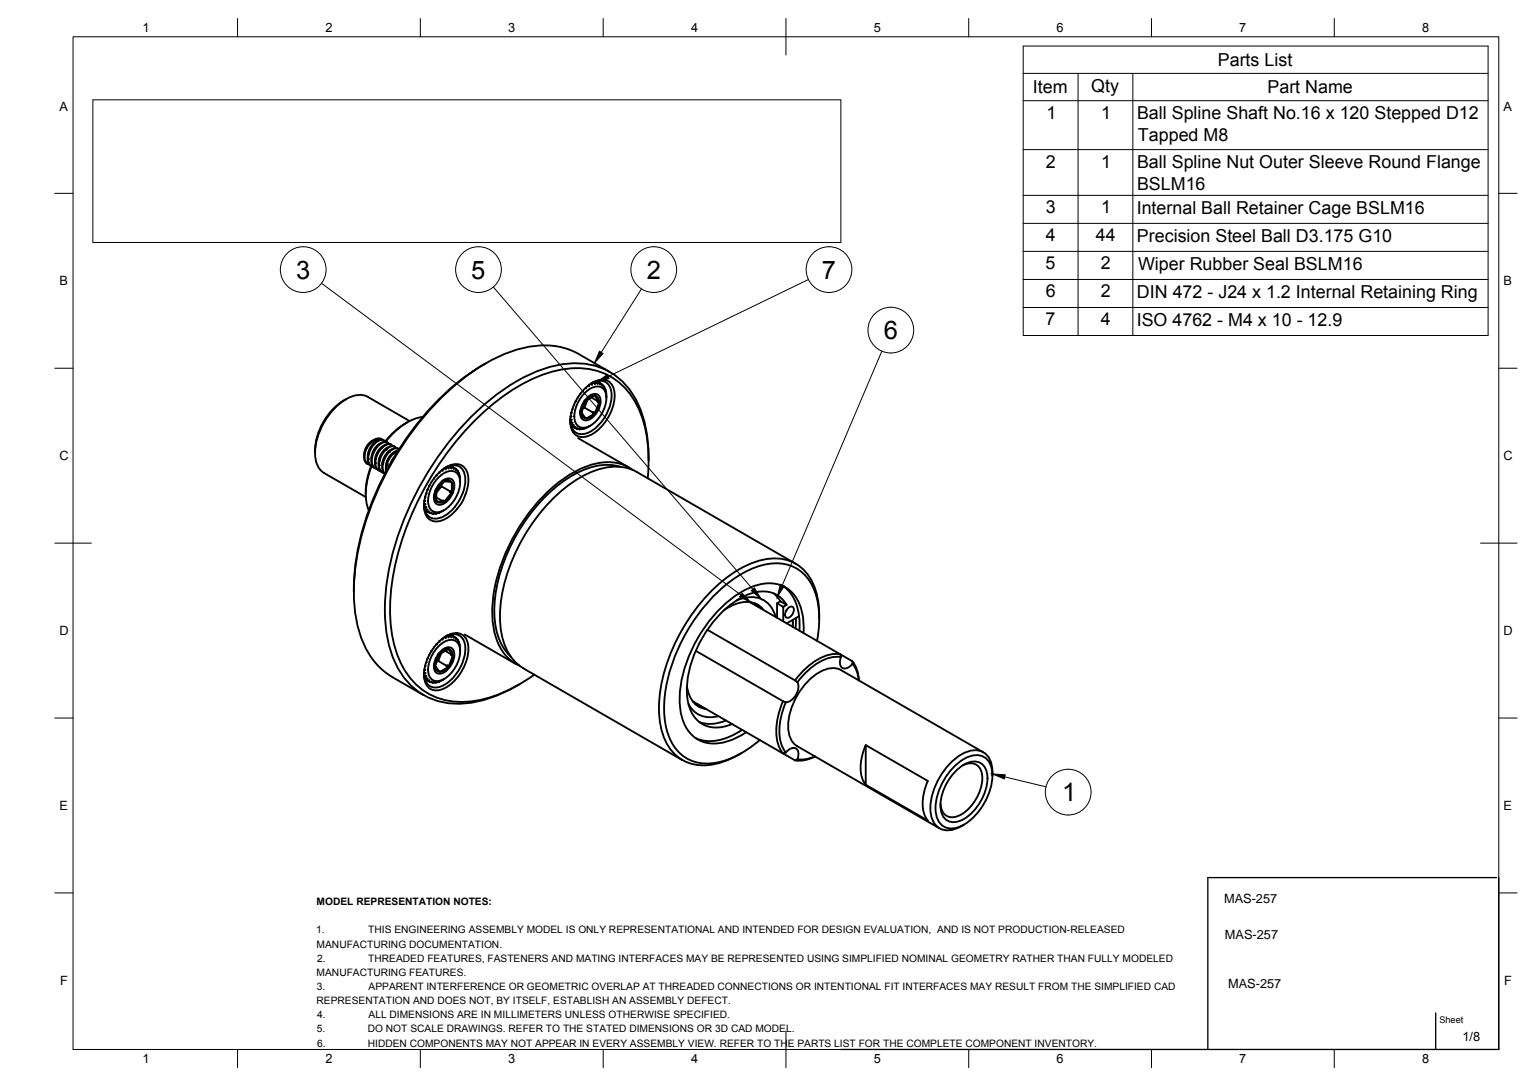
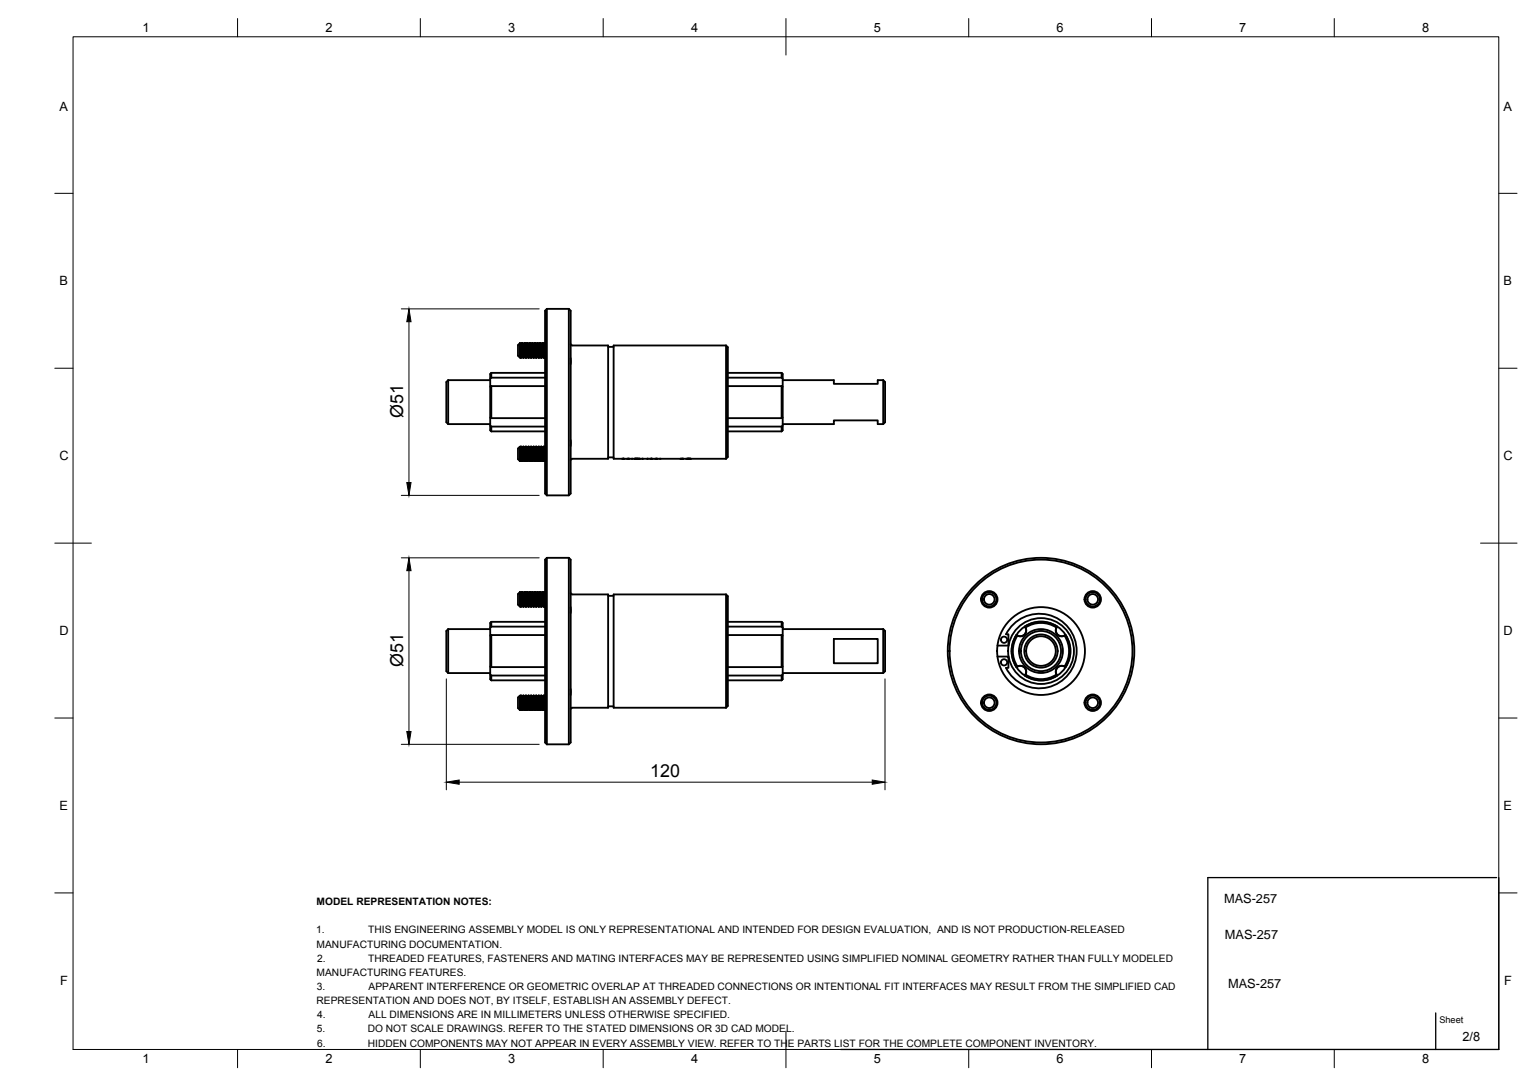
ISO-10303-21;
HEADER;
FILE_DESCRIPTION((''),'2;1');
FILE_NAME('MAS-257','2026-10-05T22:33:56+05:00',(''),(''),'','','');
FILE_SCHEMA (('AUTOMOTIVE_DESIGN { 1 0 10303 214 3 1 1 }'));
ENDSEC;
DATA;
#10 = MECHANICAL_DESIGN_GEOMETRIC_PRESENTATION_REPRESENTATION('',(#429,#430,
#431,#432,#433,#434,#435),#16942) ;
#11 = ITEM_DEFINED_TRANSFORMATION($,$,#8264,#8917) ;
#12 = ITEM_DEFINED_TRANSFORMATION($,$,#8345,#8918) ;
#13 = ITEM_DEFINED_TRANSFORMATION($,$,#8552,#8919) ;
#14 = ITEM_DEFINED_TRANSFORMATION($,$,#8593,#8920) ;
#15 = ITEM_DEFINED_TRANSFORMATION($,$,#8877,#8921) ;
#16 = ITEM_DEFINED_TRANSFORMATION($,$,#8896,#8922) ;
#17 = ITEM_DEFINED_TRANSFORMATION($,$,#8596,#8923) ;
#18 = ITEM_DEFINED_TRANSFORMATION($,$,#8593,#8924) ;
#19 = ITEM_DEFINED_TRANSFORMATION($,$,#8593,#8925) ;
#20 = ITEM_DEFINED_TRANSFORMATION($,$,#8593,#8926) ;
#21 = ITEM_DEFINED_TRANSFORMATION($,$,#8593,#8927) ;
#22 = ITEM_DEFINED_TRANSFORMATION($,$,#8593,#8928) ;
#23 = ITEM_DEFINED_TRANSFORMATION($,$,#8593,#8929) ;
#24 = ITEM_DEFINED_TRANSFORMATION($,$,#8593,#8930) ;
#25 = ITEM_DEFINED_TRANSFORMATION($,$,#8593,#8931) ;
#26 = ITEM_DEFINED_TRANSFORMATION($,$,#8593,#8932) ;
#27 = ITEM_DEFINED_TRANSFORMATION($,$,#8593,#8933) ;
#28 = ITEM_DEFINED_TRANSFORMATION($,$,#8593,#8934) ;
#29 = ITEM_DEFINED_TRANSFORMATION($,$,#8593,#8935) ;
#30 = ITEM_DEFINED_TRANSFORMATION($,$,#8593,#8936) ;
#31 = ITEM_DEFINED_TRANSFORMATION($,$,#8593,#8937) ;
#32 = ITEM_DEFINED_TRANSFORMATION($,$,#8593,#8938) ;
#33 = ITEM_DEFINED_TRANSFORMATION($,$,#8593,#8939) ;
#34 = ITEM_DEFINED_TRANSFORMATION($,$,#8593,#8940) ;
#35 = ITEM_DEFINED_TRANSFORMATION($,$,#8593,#8941) ;
#36 = ITEM_DEFINED_TRANSFORMATION($,$,#8593,#8942) ;
#37 = ITEM_DEFINED_TRANSFORMATION($,$,#8593,#8943) ;
#38 = ITEM_DEFINED_TRANSFORMATION($,$,#8593,#8944) ;
#39 = ITEM_DEFINED_TRANSFORMATION($,$,#8593,#8945) ;
#40 = ITEM_DEFINED_TRANSFORMATION($,$,#8593,#8946) ;
#41 = ITEM_DEFINED_TRANSFORMATION($,$,#8593,#8947) ;
#42 = ITEM_DEFINED_TRANSFORMATION($,$,#8593,#8948) ;
#43 = ITEM_DEFINED_TRANSFORMATION($,$,#8593,#8949) ;
#44 = ITEM_DEFINED_TRANSFORMATION($,$,#8593,#8950) ;
#45 = ITEM_DEFINED_TRANSFORMATION($,$,#8593,#8951) ;
#46 = ITEM_DEFINED_TRANSFORMATION($,$,#8593,#8952) ;
#47 = ITEM_DEFINED_TRANSFORMATION($,$,#8593,#8953) ;
#48 = ITEM_DEFINED_TRANSFORMATION($,$,#8593,#8954) ;
#49 = ITEM_DEFINED_TRANSFORMATION($,$,#8593,#8955) ;
#50 = ITEM_DEFINED_TRANSFORMATION($,$,#8593,#8956) ;
#51 = ITEM_DEFINED_TRANSFORMATION($,$,#8593,#8957) ;
#52 = ITEM_DEFINED_TRANSFORMATION($,$,#8593,#8958) ;
#53 = ITEM_DEFINED_TRANSFORMATION($,$,#8593,#8959) ;
#54 = ITEM_DEFINED_TRANSFORMATION($,$,#8593,#8960) ;
#55 = ITEM_DEFINED_TRANSFORMATION($,$,#8593,#8961) ;
#56 = ITEM_DEFINED_TRANSFORMATION($,$,#8593,#8962) ;
#57 = ITEM_DEFINED_TRANSFORMATION($,$,#8593,#8963) ;
#58 = ITEM_DEFINED_TRANSFORMATION($,$,#8593,#8964) ;
#59 = ITEM_DEFINED_TRANSFORMATION($,$,#8593,#8965) ;
#60 = ITEM_DEFINED_TRANSFORMATION($,$,#8593,#8966) ;
#61 = ITEM_DEFINED_TRANSFORMATION($,$,#8596,#8967) ;
#62 = ITEM_DEFINED_TRANSFORMATION($,$,#8596,#8968) ;
#63 = ITEM_DEFINED_TRANSFORMATION($,$,#8596,#8969) ;
#64 = ITEM_DEFINED_TRANSFORMATION($,$,#8877,#8970) ;
#65 = ITEM_DEFINED_TRANSFORMATION($,$,#8896,#8971) ;
#66 = (
REPRESENTATION_RELATIONSHIP($,$,#17019,#17018)
REPRESENTATION_RELATIONSHIP_WITH_TRANSFORMATION(#11)
SHAPE_REPRESENTATION_RELATIONSHIP()
) ;
#67 = (
REPRESENTATION_RELATIONSHIP($,$,#17020,#17018)
REPRESENTATION_RELATIONSHIP_WITH_TRANSFORMATION(#12)
SHAPE_REPRESENTATION_RELATIONSHIP()
) ;
#68 = (
REPRESENTATION_RELATIONSHIP($,$,#17021,#17018)
REPRESENTATION_RELATIONSHIP_WITH_TRANSFORMATION(#13)
SHAPE_REPRESENTATION_RELATIONSHIP()
) ;
#69 = (
REPRESENTATION_RELATIONSHIP($,$,#17022,#17018)
REPRESENTATION_RELATIONSHIP_WITH_TRANSFORMATION(#14)
SHAPE_REPRESENTATION_RELATIONSHIP()
) ;
#70 = (
REPRESENTATION_RELATIONSHIP($,$,#17024,#17018)
REPRESENTATION_RELATIONSHIP_WITH_TRANSFORMATION(#15)
SHAPE_REPRESENTATION_RELATIONSHIP()
) ;
#71 = (
REPRESENTATION_RELATIONSHIP($,$,#17025,#17018)
REPRESENTATION_RELATIONSHIP_WITH_TRANSFORMATION(#16)
SHAPE_REPRESENTATION_RELATIONSHIP()
) ;
#72 = (
REPRESENTATION_RELATIONSHIP($,$,#17023,#17018)
REPRESENTATION_RELATIONSHIP_WITH_TRANSFORMATION(#17)
SHAPE_REPRESENTATION_RELATIONSHIP()
) ;
#73 = (
REPRESENTATION_RELATIONSHIP($,$,#17022,#17018)
REPRESENTATION_RELATIONSHIP_WITH_TRANSFORMATION(#18)
SHAPE_REPRESENTATION_RELATIONSHIP()
) ;
#74 = (
REPRESENTATION_RELATIONSHIP($,$,#17022,#17018)
REPRESENTATION_RELATIONSHIP_WITH_TRANSFORMATION(#19)
SHAPE_REPRESENTATION_RELATIONSHIP()
) ;
#75 = (
REPRESENTATION_RELATIONSHIP($,$,#17022,#17018)
REPRESENTATION_RELATIONSHIP_WITH_TRANSFORMATION(#20)
SHAPE_REPRESENTATION_RELATIONSHIP()
) ;
#76 = (
REPRESENTATION_RELATIONSHIP($,$,#17022,#17018)
REPRESENTATION_RELATIONSHIP_WITH_TRANSFORMATION(#21)
SHAPE_REPRESENTATION_RELATIONSHIP()
) ;
#77 = (
REPRESENTATION_RELATIONSHIP($,$,#17022,#17018)
REPRESENTATION_RELATIONSHIP_WITH_TRANSFORMATION(#22)
SHAPE_REPRESENTATION_RELATIONSHIP()
) ;
#78 = (
REPRESENTATION_RELATIONSHIP($,$,#17022,#17018)
REPRESENTATION_RELATIONSHIP_WITH_TRANSFORMATION(#23)
SHAPE_REPRESENTATION_RELATIONSHIP()
) ;
#79 = (
REPRESENTATION_RELATIONSHIP($,$,#17022,#17018)
REPRESENTATION_RELATIONSHIP_WITH_TRANSFORMATION(#24)
SHAPE_REPRESENTATION_RELATIONSHIP()
) ;
#80 = (
REPRESENTATION_RELATIONSHIP($,$,#17022,#17018)
REPRESENTATION_RELATIONSHIP_WITH_TRANSFORMATION(#25)
SHAPE_REPRESENTATION_RELATIONSHIP()
) ;
#81 = (
REPRESENTATION_RELATIONSHIP($,$,#17022,#17018)
REPRESENTATION_RELATIONSHIP_WITH_TRANSFORMATION(#26)
SHAPE_REPRESENTATION_RELATIONSHIP()
) ;
#82 = (
REPRESENTATION_RELATIONSHIP($,$,#17022,#17018)
REPRESENTATION_RELATIONSHIP_WITH_TRANSFORMATION(#27)
SHAPE_REPRESENTATION_RELATIONSHIP()
) ;
#83 = (
REPRESENTATION_RELATIONSHIP($,$,#17022,#17018)
REPRESENTATION_RELATIONSHIP_WITH_TRANSFORMATION(#28)
SHAPE_REPRESENTATION_RELATIONSHIP()
) ;
#84 = (
REPRESENTATION_RELATIONSHIP($,$,#17022,#17018)
REPRESENTATION_RELATIONSHIP_WITH_TRANSFORMATION(#29)
SHAPE_REPRESENTATION_RELATIONSHIP()
) ;
#85 = (
REPRESENTATION_RELATIONSHIP($,$,#17022,#17018)
REPRESENTATION_RELATIONSHIP_WITH_TRANSFORMATION(#30)
SHAPE_REPRESENTATION_RELATIONSHIP()
) ;
#86 = (
REPRESENTATION_RELATIONSHIP($,$,#17022,#17018)
REPRESENTATION_RELATIONSHIP_WITH_TRANSFORMATION(#31)
SHAPE_REPRESENTATION_RELATIONSHIP()
) ;
#87 = (
REPRESENTATION_RELATIONSHIP($,$,#17022,#17018)
REPRESENTATION_RELATIONSHIP_WITH_TRANSFORMATION(#32)
SHAPE_REPRESENTATION_RELATIONSHIP()
) ;
#88 = (
REPRESENTATION_RELATIONSHIP($,$,#17022,#17018)
REPRESENTATION_RELATIONSHIP_WITH_TRANSFORMATION(#33)
SHAPE_REPRESENTATION_RELATIONSHIP()
) ;
#89 = (
REPRESENTATION_RELATIONSHIP($,$,#17022,#17018)
REPRESENTATION_RELATIONSHIP_WITH_TRANSFORMATION(#34)
SHAPE_REPRESENTATION_RELATIONSHIP()
) ;
#90 = (
REPRESENTATION_RELATIONSHIP($,$,#17022,#17018)
REPRESENTATION_RELATIONSHIP_WITH_TRANSFORMATION(#35)
SHAPE_REPRESENTATION_RELATIONSHIP()
) ;
#91 = (
REPRESENTATION_RELATIONSHIP($,$,#17022,#17018)
REPRESENTATION_RELATIONSHIP_WITH_TRANSFORMATION(#36)
SHAPE_REPRESENTATION_RELATIONSHIP()
) ;
#92 = (
REPRESENTATION_RELATIONSHIP($,$,#17022,#17018)
REPRESENTATION_RELATIONSHIP_WITH_TRANSFORMATION(#37)
SHAPE_REPRESENTATION_RELATIONSHIP()
) ;
#93 = (
REPRESENTATION_RELATIONSHIP($,$,#17022,#17018)
REPRESENTATION_RELATIONSHIP_WITH_TRANSFORMATION(#38)
SHAPE_REPRESENTATION_RELATIONSHIP()
) ;
#94 = (
REPRESENTATION_RELATIONSHIP($,$,#17022,#17018)
REPRESENTATION_RELATIONSHIP_WITH_TRANSFORMATION(#39)
SHAPE_REPRESENTATION_RELATIONSHIP()
) ;
#95 = (
REPRESENTATION_RELATIONSHIP($,$,#17022,#17018)
REPRESENTATION_RELATIONSHIP_WITH_TRANSFORMATION(#40)
SHAPE_REPRESENTATION_RELATIONSHIP()
) ;
#96 = (
REPRESENTATION_RELATIONSHIP($,$,#17022,#17018)
REPRESENTATION_RELATIONSHIP_WITH_TRANSFORMATION(#41)
SHAPE_REPRESENTATION_RELATIONSHIP()
) ;
#97 = (
REPRESENTATION_RELATIONSHIP($,$,#17022,#17018)
REPRESENTATION_RELATIONSHIP_WITH_TRANSFORMATION(#42)
SHAPE_REPRESENTATION_RELATIONSHIP()
) ;
#98 = (
REPRESENTATION_RELATIONSHIP($,$,#17022,#17018)
REPRESENTATION_RELATIONSHIP_WITH_TRANSFORMATION(#43)
SHAPE_REPRESENTATION_RELATIONSHIP()
) ;
#99 = (
REPRESENTATION_RELATIONSHIP($,$,#17022,#17018)
REPRESENTATION_RELATIONSHIP_WITH_TRANSFORMATION(#44)
SHAPE_REPRESENTATION_RELATIONSHIP()
) ;
#100 = (
REPRESENTATION_RELATIONSHIP($,$,#17022,#17018)
REPRESENTATION_RELATIONSHIP_WITH_TRANSFORMATION(#45)
SHAPE_REPRESENTATION_RELATIONSHIP()
) ;
#101 = (
REPRESENTATION_RELATIONSHIP($,$,#17022,#17018)
REPRESENTATION_RELATIONSHIP_WITH_TRANSFORMATION(#46)
SHAPE_REPRESENTATION_RELATIONSHIP()
) ;
#102 = (
REPRESENTATION_RELATIONSHIP($,$,#17022,#17018)
REPRESENTATION_RELATIONSHIP_WITH_TRANSFORMATION(#47)
SHAPE_REPRESENTATION_RELATIONSHIP()
) ;
#103 = (
REPRESENTATION_RELATIONSHIP($,$,#17022,#17018)
REPRESENTATION_RELATIONSHIP_WITH_TRANSFORMATION(#48)
SHAPE_REPRESENTATION_RELATIONSHIP()
) ;
#104 = (
REPRESENTATION_RELATIONSHIP($,$,#17022,#17018)
REPRESENTATION_RELATIONSHIP_WITH_TRANSFORMATION(#49)
SHAPE_REPRESENTATION_RELATIONSHIP()
) ;
#105 = (
REPRESENTATION_RELATIONSHIP($,$,#17022,#17018)
REPRESENTATION_RELATIONSHIP_WITH_TRANSFORMATION(#50)
SHAPE_REPRESENTATION_RELATIONSHIP()
) ;
#106 = (
REPRESENTATION_RELATIONSHIP($,$,#17022,#17018)
REPRESENTATION_RELATIONSHIP_WITH_TRANSFORMATION(#51)
SHAPE_REPRESENTATION_RELATIONSHIP()
) ;
#107 = (
REPRESENTATION_RELATIONSHIP($,$,#17022,#17018)
REPRESENTATION_RELATIONSHIP_WITH_TRANSFORMATION(#52)
SHAPE_REPRESENTATION_RELATIONSHIP()
) ;
#108 = (
REPRESENTATION_RELATIONSHIP($,$,#17022,#17018)
REPRESENTATION_RELATIONSHIP_WITH_TRANSFORMATION(#53)
SHAPE_REPRESENTATION_RELATIONSHIP()
) ;
#109 = (
REPRESENTATION_RELATIONSHIP($,$,#17022,#17018)
REPRESENTATION_RELATIONSHIP_WITH_TRANSFORMATION(#54)
SHAPE_REPRESENTATION_RELATIONSHIP()
) ;
#110 = (
REPRESENTATION_RELATIONSHIP($,$,#17022,#17018)
REPRESENTATION_RELATIONSHIP_WITH_TRANSFORMATION(#55)
SHAPE_REPRESENTATION_RELATIONSHIP()
) ;
#111 = (
REPRESENTATION_RELATIONSHIP($,$,#17022,#17018)
REPRESENTATION_RELATIONSHIP_WITH_TRANSFORMATION(#56)
SHAPE_REPRESENTATION_RELATIONSHIP()
) ;
#112 = (
REPRESENTATION_RELATIONSHIP($,$,#17022,#17018)
REPRESENTATION_RELATIONSHIP_WITH_TRANSFORMATION(#57)
SHAPE_REPRESENTATION_RELATIONSHIP()
) ;
#113 = (
REPRESENTATION_RELATIONSHIP($,$,#17022,#17018)
REPRESENTATION_RELATIONSHIP_WITH_TRANSFORMATION(#58)
SHAPE_REPRESENTATION_RELATIONSHIP()
) ;
#114 = (
REPRESENTATION_RELATIONSHIP($,$,#17022,#17018)
REPRESENTATION_RELATIONSHIP_WITH_TRANSFORMATION(#59)
SHAPE_REPRESENTATION_RELATIONSHIP()
) ;
#115 = (
REPRESENTATION_RELATIONSHIP($,$,#17022,#17018)
REPRESENTATION_RELATIONSHIP_WITH_TRANSFORMATION(#60)
SHAPE_REPRESENTATION_RELATIONSHIP()
) ;
#116 = (
REPRESENTATION_RELATIONSHIP($,$,#17023,#17018)
REPRESENTATION_RELATIONSHIP_WITH_TRANSFORMATION(#61)
SHAPE_REPRESENTATION_RELATIONSHIP()
) ;
#117 = (
REPRESENTATION_RELATIONSHIP($,$,#17023,#17018)
REPRESENTATION_RELATIONSHIP_WITH_TRANSFORMATION(#62)
SHAPE_REPRESENTATION_RELATIONSHIP()
) ;
#118 = (
REPRESENTATION_RELATIONSHIP($,$,#17023,#17018)
REPRESENTATION_RELATIONSHIP_WITH_TRANSFORMATION(#63)
SHAPE_REPRESENTATION_RELATIONSHIP()
) ;
#119 = (
REPRESENTATION_RELATIONSHIP($,$,#17024,#17018)
REPRESENTATION_RELATIONSHIP_WITH_TRANSFORMATION(#64)
SHAPE_REPRESENTATION_RELATIONSHIP()
) ;
#120 = (
REPRESENTATION_RELATIONSHIP($,$,#17025,#17018)
REPRESENTATION_RELATIONSHIP_WITH_TRANSFORMATION(#65)
SHAPE_REPRESENTATION_RELATIONSHIP()
) ;
#121 = CONTEXT_DEPENDENT_SHAPE_REPRESENTATION(#66,#16963) ;
#122 = CONTEXT_DEPENDENT_SHAPE_REPRESENTATION(#67,#16964) ;
#123 = CONTEXT_DEPENDENT_SHAPE_REPRESENTATION(#68,#16965) ;
#124 = CONTEXT_DEPENDENT_SHAPE_REPRESENTATION(#69,#16966) ;
#125 = CONTEXT_DEPENDENT_SHAPE_REPRESENTATION(#70,#16967) ;
#126 = CONTEXT_DEPENDENT_SHAPE_REPRESENTATION(#71,#16968) ;
#127 = CONTEXT_DEPENDENT_SHAPE_REPRESENTATION(#72,#16969) ;
#128 = CONTEXT_DEPENDENT_SHAPE_REPRESENTATION(#73,#16970) ;
#129 = CONTEXT_DEPENDENT_SHAPE_REPRESENTATION(#74,#16971) ;
#130 = CONTEXT_DEPENDENT_SHAPE_REPRESENTATION(#75,#16972) ;
#131 = CONTEXT_DEPENDENT_SHAPE_REPRESENTATION(#76,#16973) ;
#132 = CONTEXT_DEPENDENT_SHAPE_REPRESENTATION(#77,#16974) ;
#133 = CONTEXT_DEPENDENT_SHAPE_REPRESENTATION(#78,#16975) ;
#134 = CONTEXT_DEPENDENT_SHAPE_REPRESENTATION(#79,#16976) ;
#135 = CONTEXT_DEPENDENT_SHAPE_REPRESENTATION(#80,#16977) ;
#136 = CONTEXT_DEPENDENT_SHAPE_REPRESENTATION(#81,#16978) ;
#137 = CONTEXT_DEPENDENT_SHAPE_REPRESENTATION(#82,#16979) ;
#138 = CONTEXT_DEPENDENT_SHAPE_REPRESENTATION(#83,#16980) ;
#139 = CONTEXT_DEPENDENT_SHAPE_REPRESENTATION(#84,#16981) ;
#140 = CONTEXT_DEPENDENT_SHAPE_REPRESENTATION(#85,#16982) ;
#141 = CONTEXT_DEPENDENT_SHAPE_REPRESENTATION(#86,#16983) ;
#142 = CONTEXT_DEPENDENT_SHAPE_REPRESENTATION(#87,#16984) ;
#143 = CONTEXT_DEPENDENT_SHAPE_REPRESENTATION(#88,#16985) ;
#144 = CONTEXT_DEPENDENT_SHAPE_REPRESENTATION(#89,#16986) ;
#145 = CONTEXT_DEPENDENT_SHAPE_REPRESENTATION(#90,#16987) ;
#146 = CONTEXT_DEPENDENT_SHAPE_REPRESENTATION(#91,#16988) ;
#147 = CONTEXT_DEPENDENT_SHAPE_REPRESENTATION(#92,#16989) ;
#148 = CONTEXT_DEPENDENT_SHAPE_REPRESENTATION(#93,#16990) ;
#149 = CONTEXT_DEPENDENT_SHAPE_REPRESENTATION(#94,#16991) ;
#150 = CONTEXT_DEPENDENT_SHAPE_REPRESENTATION(#95,#16992) ;
#151 = CONTEXT_DEPENDENT_SHAPE_REPRESENTATION(#96,#16993) ;
#152 = CONTEXT_DEPENDENT_SHAPE_REPRESENTATION(#97,#16994) ;
#153 = CONTEXT_DEPENDENT_SHAPE_REPRESENTATION(#98,#16995) ;
#154 = CONTEXT_DEPENDENT_SHAPE_REPRESENTATION(#99,#16996) ;
#155 = CONTEXT_DEPENDENT_SHAPE_REPRESENTATION(#100,#16997) ;
#156 = CONTEXT_DEPENDENT_SHAPE_REPRESENTATION(#101,#16998) ;
#157 = CONTEXT_DEPENDENT_SHAPE_REPRESENTATION(#102,#16999) ;
#158 = CONTEXT_DEPENDENT_SHAPE_REPRESENTATION(#103,#17000) ;
#159 = CONTEXT_DEPENDENT_SHAPE_REPRESENTATION(#104,#17001) ;
#160 = CONTEXT_DEPENDENT_SHAPE_REPRESENTATION(#105,#17002) ;
#161 = CONTEXT_DEPENDENT_SHAPE_REPRESENTATION(#106,#17003) ;
#162 = CONTEXT_DEPENDENT_SHAPE_REPRESENTATION(#107,#17004) ;
#163 = CONTEXT_DEPENDENT_SHAPE_REPRESENTATION(#108,#17005) ;
#164 = CONTEXT_DEPENDENT_SHAPE_REPRESENTATION(#109,#17006) ;
#165 = CONTEXT_DEPENDENT_SHAPE_REPRESENTATION(#110,#17007) ;
#166 = CONTEXT_DEPENDENT_SHAPE_REPRESENTATION(#111,#17008) ;
#167 = CONTEXT_DEPENDENT_SHAPE_REPRESENTATION(#112,#17009) ;
#168 = CONTEXT_DEPENDENT_SHAPE_REPRESENTATION(#113,#17010) ;
#169 = CONTEXT_DEPENDENT_SHAPE_REPRESENTATION(#114,#17011) ;
#170 = CONTEXT_DEPENDENT_SHAPE_REPRESENTATION(#115,#17012) ;
#171 = CONTEXT_DEPENDENT_SHAPE_REPRESENTATION(#116,#17013) ;
#172 = CONTEXT_DEPENDENT_SHAPE_REPRESENTATION(#117,#17014) ;
#173 = CONTEXT_DEPENDENT_SHAPE_REPRESENTATION(#118,#17015) ;
#174 = CONTEXT_DEPENDENT_SHAPE_REPRESENTATION(#119,#17016) ;
#175 = CONTEXT_DEPENDENT_SHAPE_REPRESENTATION(#120,#17017) ;
#176 = NEXT_ASSEMBLY_USAGE_OCCURRENCE(
'Ball Spline Shaft No.16 x 120 Stepped D12 Tapped M8:1',
'Ball Spline Shaft No.16 x 120 Stepped D12 Tapped M8:1',
'Ball Spline Shaft No.16 x 120 Stepped D12 Tapped M8:1',#17027,#17028,
'Ball Spline Shaft No.16 x 120 Stepped D12 Tapped M8:1') ;
#177 = NEXT_ASSEMBLY_USAGE_OCCURRENCE(
'Ball Spline Nut Outer Sleeve Round Flange BSLM16:1',
'Ball Spline Nut Outer Sleeve Round Flange BSLM16:1',
'Ball Spline Nut Outer Sleeve Round Flange BSLM16:1',#17027,#17029,
'Ball Spline Nut Outer Sleeve Round Flange BSLM16:1') ;
#178 = NEXT_ASSEMBLY_USAGE_OCCURRENCE(
'Internal Ball Retainer Cage BSLM16:1',
'Internal Ball Retainer Cage BSLM16:1',
'Internal Ball Retainer Cage BSLM16:1',#17027,#17030,
'Internal Ball Retainer Cage BSLM16:1') ;
#179 = NEXT_ASSEMBLY_USAGE_OCCURRENCE('Precision Steel Ball D3.175 G10:1',
'Precision Steel Ball D3.175 G10:1','Precision Steel Ball D3.175 G10:1',
#17027,#17031,'Precision Steel Ball D3.175 G10:1') ;
#180 = NEXT_ASSEMBLY_USAGE_OCCURRENCE('Wiper Rubber Seal BSLM16:1',
'Wiper Rubber Seal BSLM16:1','Wiper Rubber Seal BSLM16:1',#17027,#17033,
'Wiper Rubber Seal BSLM16:1') ;
#181 = NEXT_ASSEMBLY_USAGE_OCCURRENCE(
'DIN 472 - J24 x 1.2 Internal Retaining Ring:1',
'DIN 472 - J24 x 1.2 Internal Retaining Ring:1',
'DIN 472 - J24 x 1.2 Internal Retaining Ring:1',#17027,#17034,
'DIN 472 - J24 x 1.2 Internal Retaining Ring:1') ;
#182 = NEXT_ASSEMBLY_USAGE_OCCURRENCE('ISO 4762 - M4 x 10 - 12.9:1',
'ISO 4762 - M4 x 10 - 12.9:1','ISO 4762 - M4 x 10 - 12.9:1',#17027,#17032,
'ISO 4762 - M4 x 10 - 12.9:1') ;
#183 = NEXT_ASSEMBLY_USAGE_OCCURRENCE('Precision Steel Ball D3.175 G10:2',
'Precision Steel Ball D3.175 G10:2','Precision Steel Ball D3.175 G10:2',
#17027,#17031,'Precision Steel Ball D3.175 G10:2') ;
#184 = NEXT_ASSEMBLY_USAGE_OCCURRENCE('Precision Steel Ball D3.175 G10:3',
'Precision Steel Ball D3.175 G10:3','Precision Steel Ball D3.175 G10:3',
#17027,#17031,'Precision Steel Ball D3.175 G10:3') ;
#185 = NEXT_ASSEMBLY_USAGE_OCCURRENCE('Precision Steel Ball D3.175 G10:4',
'Precision Steel Ball D3.175 G10:4','Precision Steel Ball D3.175 G10:4',
#17027,#17031,'Precision Steel Ball D3.175 G10:4') ;
#186 = NEXT_ASSEMBLY_USAGE_OCCURRENCE('Precision Steel Ball D3.175 G10:5',
'Precision Steel Ball D3.175 G10:5','Precision Steel Ball D3.175 G10:5',
#17027,#17031,'Precision Steel Ball D3.175 G10:5') ;
#187 = NEXT_ASSEMBLY_USAGE_OCCURRENCE('Precision Steel Ball D3.175 G10:6',
'Precision Steel Ball D3.175 G10:6','Precision Steel Ball D3.175 G10:6',
#17027,#17031,'Precision Steel Ball D3.175 G10:6') ;
#188 = NEXT_ASSEMBLY_USAGE_OCCURRENCE('Precision Steel Ball D3.175 G10:7',
'Precision Steel Ball D3.175 G10:7','Precision Steel Ball D3.175 G10:7',
#17027,#17031,'Precision Steel Ball D3.175 G10:7') ;
#189 = NEXT_ASSEMBLY_USAGE_OCCURRENCE('Precision Steel Ball D3.175 G10:8',
'Precision Steel Ball D3.175 G10:8','Precision Steel Ball D3.175 G10:8',
#17027,#17031,'Precision Steel Ball D3.175 G10:8') ;
#190 = NEXT_ASSEMBLY_USAGE_OCCURRENCE('Precision Steel Ball D3.175 G10:9',
'Precision Steel Ball D3.175 G10:9','Precision Steel Ball D3.175 G10:9',
#17027,#17031,'Precision Steel Ball D3.175 G10:9') ;
#191 = NEXT_ASSEMBLY_USAGE_OCCURRENCE(
'Precision Steel Ball D3.175 G10:10',
'Precision Steel Ball D3.175 G10:10',
'Precision Steel Ball D3.175 G10:10',#17027,#17031,
'Precision Steel Ball D3.175 G10:10') ;
#192 = NEXT_ASSEMBLY_USAGE_OCCURRENCE(
'Precision Steel Ball D3.175 G10:11',
'Precision Steel Ball D3.175 G10:11',
'Precision Steel Ball D3.175 G10:11',#17027,#17031,
'Precision Steel Ball D3.175 G10:11') ;
#193 = NEXT_ASSEMBLY_USAGE_OCCURRENCE(
'Precision Steel Ball D3.175 G10:12',
'Precision Steel Ball D3.175 G10:12',
'Precision Steel Ball D3.175 G10:12',#17027,#17031,
'Precision Steel Ball D3.175 G10:12') ;
#194 = NEXT_ASSEMBLY_USAGE_OCCURRENCE(
'Precision Steel Ball D3.175 G10:13',
'Precision Steel Ball D3.175 G10:13',
'Precision Steel Ball D3.175 G10:13',#17027,#17031,
'Precision Steel Ball D3.175 G10:13') ;
#195 = NEXT_ASSEMBLY_USAGE_OCCURRENCE(
'Precision Steel Ball D3.175 G10:14',
'Precision Steel Ball D3.175 G10:14',
'Precision Steel Ball D3.175 G10:14',#17027,#17031,
'Precision Steel Ball D3.175 G10:14') ;
#196 = NEXT_ASSEMBLY_USAGE_OCCURRENCE(
'Precision Steel Ball D3.175 G10:15',
'Precision Steel Ball D3.175 G10:15',
'Precision Steel Ball D3.175 G10:15',#17027,#17031,
'Precision Steel Ball D3.175 G10:15') ;
#197 = NEXT_ASSEMBLY_USAGE_OCCURRENCE(
'Precision Steel Ball D3.175 G10:16',
'Precision Steel Ball D3.175 G10:16',
'Precision Steel Ball D3.175 G10:16',#17027,#17031,
'Precision Steel Ball D3.175 G10:16') ;
#198 = NEXT_ASSEMBLY_USAGE_OCCURRENCE(
'Precision Steel Ball D3.175 G10:17',
'Precision Steel Ball D3.175 G10:17',
'Precision Steel Ball D3.175 G10:17',#17027,#17031,
'Precision Steel Ball D3.175 G10:17') ;
#199 = NEXT_ASSEMBLY_USAGE_OCCURRENCE(
'Precision Steel Ball D3.175 G10:18',
'Precision Steel Ball D3.175 G10:18',
'Precision Steel Ball D3.175 G10:18',#17027,#17031,
'Precision Steel Ball D3.175 G10:18') ;
#200 = NEXT_ASSEMBLY_USAGE_OCCURRENCE(
'Precision Steel Ball D3.175 G10:19',
'Precision Steel Ball D3.175 G10:19',
'Precision Steel Ball D3.175 G10:19',#17027,#17031,
'Precision Steel Ball D3.175 G10:19') ;
#201 = NEXT_ASSEMBLY_USAGE_OCCURRENCE(
'Precision Steel Ball D3.175 G10:20',
'Precision Steel Ball D3.175 G10:20',
'Precision Steel Ball D3.175 G10:20',#17027,#17031,
'Precision Steel Ball D3.175 G10:20') ;
#202 = NEXT_ASSEMBLY_USAGE_OCCURRENCE(
'Precision Steel Ball D3.175 G10:21',
'Precision Steel Ball D3.175 G10:21',
'Precision Steel Ball D3.175 G10:21',#17027,#17031,
'Precision Steel Ball D3.175 G10:21') ;
#203 = NEXT_ASSEMBLY_USAGE_OCCURRENCE(
'Precision Steel Ball D3.175 G10:22',
'Precision Steel Ball D3.175 G10:22',
'Precision Steel Ball D3.175 G10:22',#17027,#17031,
'Precision Steel Ball D3.175 G10:22') ;
#204 = NEXT_ASSEMBLY_USAGE_OCCURRENCE(
'Precision Steel Ball D3.175 G10:23',
'Precision Steel Ball D3.175 G10:23',
'Precision Steel Ball D3.175 G10:23',#17027,#17031,
'Precision Steel Ball D3.175 G10:23') ;
#205 = NEXT_ASSEMBLY_USAGE_OCCURRENCE(
'Precision Steel Ball D3.175 G10:24',
'Precision Steel Ball D3.175 G10:24',
'Precision Steel Ball D3.175 G10:24',#17027,#17031,
'Precision Steel Ball D3.175 G10:24') ;
#206 = NEXT_ASSEMBLY_USAGE_OCCURRENCE(
'Precision Steel Ball D3.175 G10:25',
'Precision Steel Ball D3.175 G10:25',
'Precision Steel Ball D3.175 G10:25',#17027,#17031,
'Precision Steel Ball D3.175 G10:25') ;
#207 = NEXT_ASSEMBLY_USAGE_OCCURRENCE(
'Precision Steel Ball D3.175 G10:26',
'Precision Steel Ball D3.175 G10:26',
'Precision Steel Ball D3.175 G10:26',#17027,#17031,
'Precision Steel Ball D3.175 G10:26') ;
#208 = NEXT_ASSEMBLY_USAGE_OCCURRENCE(
'Precision Steel Ball D3.175 G10:27',
'Precision Steel Ball D3.175 G10:27',
'Precision Steel Ball D3.175 G10:27',#17027,#17031,
'Precision Steel Ball D3.175 G10:27') ;
#209 = NEXT_ASSEMBLY_USAGE_OCCURRENCE(
'Precision Steel Ball D3.175 G10:28',
'Precision Steel Ball D3.175 G10:28',
'Precision Steel Ball D3.175 G10:28',#17027,#17031,
'Precision Steel Ball D3.175 G10:28') ;
#210 = NEXT_ASSEMBLY_USAGE_OCCURRENCE(
'Precision Steel Ball D3.175 G10:29',
'Precision Steel Ball D3.175 G10:29',
'Precision Steel Ball D3.175 G10:29',#17027,#17031,
'Precision Steel Ball D3.175 G10:29') ;
#211 = NEXT_ASSEMBLY_USAGE_OCCURRENCE(
'Precision Steel Ball D3.175 G10:30',
'Precision Steel Ball D3.175 G10:30',
'Precision Steel Ball D3.175 G10:30',#17027,#17031,
'Precision Steel Ball D3.175 G10:30') ;
#212 = NEXT_ASSEMBLY_USAGE_OCCURRENCE(
'Precision Steel Ball D3.175 G10:31',
'Precision Steel Ball D3.175 G10:31',
'Precision Steel Ball D3.175 G10:31',#17027,#17031,
'Precision Steel Ball D3.175 G10:31') ;
#213 = NEXT_ASSEMBLY_USAGE_OCCURRENCE(
'Precision Steel Ball D3.175 G10:32',
'Precision Steel Ball D3.175 G10:32',
'Precision Steel Ball D3.175 G10:32',#17027,#17031,
'Precision Steel Ball D3.175 G10:32') ;
#214 = NEXT_ASSEMBLY_USAGE_OCCURRENCE(
'Precision Steel Ball D3.175 G10:33',
'Precision Steel Ball D3.175 G10:33',
'Precision Steel Ball D3.175 G10:33',#17027,#17031,
'Precision Steel Ball D3.175 G10:33') ;
#215 = NEXT_ASSEMBLY_USAGE_OCCURRENCE(
'Precision Steel Ball D3.175 G10:34',
'Precision Steel Ball D3.175 G10:34',
'Precision Steel Ball D3.175 G10:34',#17027,#17031,
'Precision Steel Ball D3.175 G10:34') ;
#216 = NEXT_ASSEMBLY_USAGE_OCCURRENCE(
'Precision Steel Ball D3.175 G10:35',
'Precision Steel Ball D3.175 G10:35',
'Precision Steel Ball D3.175 G10:35',#17027,#17031,
'Precision Steel Ball D3.175 G10:35') ;
#217 = NEXT_ASSEMBLY_USAGE_OCCURRENCE(
'Precision Steel Ball D3.175 G10:36',
'Precision Steel Ball D3.175 G10:36',
'Precision Steel Ball D3.175 G10:36',#17027,#17031,
'Precision Steel Ball D3.175 G10:36') ;
#218 = NEXT_ASSEMBLY_USAGE_OCCURRENCE(
'Precision Steel Ball D3.175 G10:37',
'Precision Steel Ball D3.175 G10:37',
'Precision Steel Ball D3.175 G10:37',#17027,#17031,
'Precision Steel Ball D3.175 G10:37') ;
#219 = NEXT_ASSEMBLY_USAGE_OCCURRENCE(
'Precision Steel Ball D3.175 G10:38',
'Precision Steel Ball D3.175 G10:38',
'Precision Steel Ball D3.175 G10:38',#17027,#17031,
'Precision Steel Ball D3.175 G10:38') ;
#220 = NEXT_ASSEMBLY_USAGE_OCCURRENCE(
'Precision Steel Ball D3.175 G10:39',
'Precision Steel Ball D3.175 G10:39',
'Precision Steel Ball D3.175 G10:39',#17027,#17031,
'Precision Steel Ball D3.175 G10:39') ;
#221 = NEXT_ASSEMBLY_USAGE_OCCURRENCE(
'Precision Steel Ball D3.175 G10:40',
'Precision Steel Ball D3.175 G10:40',
'Precision Steel Ball D3.175 G10:40',#17027,#17031,
'Precision Steel Ball D3.175 G10:40') ;
#222 = NEXT_ASSEMBLY_USAGE_OCCURRENCE(
'Precision Steel Ball D3.175 G10:41',
'Precision Steel Ball D3.175 G10:41',
'Precision Steel Ball D3.175 G10:41',#17027,#17031,
'Precision Steel Ball D3.175 G10:41') ;
#223 = NEXT_ASSEMBLY_USAGE_OCCURRENCE(
'Precision Steel Ball D3.175 G10:42',
'Precision Steel Ball D3.175 G10:42',
'Precision Steel Ball D3.175 G10:42',#17027,#17031,
'Precision Steel Ball D3.175 G10:42') ;
#224 = NEXT_ASSEMBLY_USAGE_OCCURRENCE(
'Precision Steel Ball D3.175 G10:43',
'Precision Steel Ball D3.175 G10:43',
'Precision Steel Ball D3.175 G10:43',#17027,#17031,
'Precision Steel Ball D3.175 G10:43') ;
#225 = NEXT_ASSEMBLY_USAGE_OCCURRENCE(
'Precision Steel Ball D3.175 G10:44',
'Precision Steel Ball D3.175 G10:44',
'Precision Steel Ball D3.175 G10:44',#17027,#17031,
'Precision Steel Ball D3.175 G10:44') ;
#226 = NEXT_ASSEMBLY_USAGE_OCCURRENCE('ISO 4762 - M4 x 10 - 12.9:2',
'ISO 4762 - M4 x 10 - 12.9:2','ISO 4762 - M4 x 10 - 12.9:2',#17027,#17032,
'ISO 4762 - M4 x 10 - 12.9:2') ;
#227 = NEXT_ASSEMBLY_USAGE_OCCURRENCE('ISO 4762 - M4 x 10 - 12.9:3',
'ISO 4762 - M4 x 10 - 12.9:3','ISO 4762 - M4 x 10 - 12.9:3',#17027,#17032,
'ISO 4762 - M4 x 10 - 12.9:3') ;
#228 = NEXT_ASSEMBLY_USAGE_OCCURRENCE('ISO 4762 - M4 x 10 - 12.9:4',
'ISO 4762 - M4 x 10 - 12.9:4','ISO 4762 - M4 x 10 - 12.9:4',#17027,#17032,
'ISO 4762 - M4 x 10 - 12.9:4') ;
#229 = NEXT_ASSEMBLY_USAGE_OCCURRENCE('Wiper Rubber Seal BSLM16:2',
'Wiper Rubber Seal BSLM16:2','Wiper Rubber Seal BSLM16:2',#17027,#17033,
'Wiper Rubber Seal BSLM16:2') ;
#230 = NEXT_ASSEMBLY_USAGE_OCCURRENCE(
'DIN 472 - J24 x 1.2 Internal Retaining Ring:2',
'DIN 472 - J24 x 1.2 Internal Retaining Ring:2',
'DIN 472 - J24 x 1.2 Internal Retaining Ring:2',#17027,#17034,
'DIN 472 - J24 x 1.2 Internal Retaining Ring:2') ;
#231 = (
BOUNDED_CURVE()
B_SPLINE_CURVE(2,(#15819,#15820,#15821),.UNSPECIFIED.,.F.,.F.)
B_SPLINE_CURVE_WITH_KNOTS((3,3),(0.0385503582642466,0.0599944283303575),
 .UNSPECIFIED.)
CURVE()
GEOMETRIC_REPRESENTATION_ITEM()
RATIONAL_B_SPLINE_CURVE((1.0010577858677,1.00082309557272,1.))
REPRESENTATION_ITEM('')
) ;
#232 = (
BOUNDED_CURVE()
B_SPLINE_CURVE(2,(#15833,#15834,#15835),.UNSPECIFIED.,.F.,.F.)
B_SPLINE_CURVE_WITH_KNOTS((3,3),(0.,0.0214440700661964),.UNSPECIFIED.)
CURVE()
GEOMETRIC_REPRESENTATION_ITEM()
RATIONAL_B_SPLINE_CURVE((1.,1.00082309556609,1.00105778585917))
REPRESENTATION_ITEM('')
) ;
#233 = (
BOUNDED_CURVE()
B_SPLINE_CURVE(2,(#16126,#16127,#16128),.UNSPECIFIED.,.F.,.F.)
B_SPLINE_CURVE_WITH_KNOTS((3,3),(0.0385503582641958,0.0599944283303579),
 .UNSPECIFIED.)
CURVE()
GEOMETRIC_REPRESENTATION_ITEM()
RATIONAL_B_SPLINE_CURVE((1.00105778586472,1.00082309557041,1.))
REPRESENTATION_ITEM('')
) ;
#234 = (
BOUNDED_CURVE()
B_SPLINE_CURVE(2,(#16135,#16136,#16137),.UNSPECIFIED.,.F.,.F.)
B_SPLINE_CURVE_WITH_KNOTS((3,3),(0.,0.0214440700661411),.UNSPECIFIED.)
CURVE()
GEOMETRIC_REPRESENTATION_ITEM()
RATIONAL_B_SPLINE_CURVE((1.,1.00082309557092,1.00105778586538))
REPRESENTATION_ITEM('')
) ;
#235 = (
BOUNDED_CURVE()
B_SPLINE_CURVE(2,(#16140,#16141,#16142),.UNSPECIFIED.,.F.,.F.)
B_SPLINE_CURVE_WITH_KNOTS((3,3),(0.0385503582642588,0.0599944283303573),
 .UNSPECIFIED.)
CURVE()
GEOMETRIC_REPRESENTATION_ITEM()
RATIONAL_B_SPLINE_CURVE((1.00105778587296,1.00082309557682,1.))
REPRESENTATION_ITEM('')
) ;
#236 = (
BOUNDED_CURVE()
B_SPLINE_CURVE(2,(#16149,#16150,#16151),.UNSPECIFIED.,.F.,.F.)
B_SPLINE_CURVE_WITH_KNOTS((3,3),(0.,0.0214440700661923),.UNSPECIFIED.)
CURVE()
GEOMETRIC_REPRESENTATION_ITEM()
RATIONAL_B_SPLINE_CURVE((1.,1.00082309556743,1.00105778586089))
REPRESENTATION_ITEM('')
) ;
#237 = (
BOUNDED_CURVE()
B_SPLINE_CURVE(2,(#16154,#16155,#16156),.UNSPECIFIED.,.F.,.F.)
B_SPLINE_CURVE_WITH_KNOTS((3,3),(0.0385503582642198,0.0599944283303572),
 .UNSPECIFIED.)
CURVE()
GEOMETRIC_REPRESENTATION_ITEM()
RATIONAL_B_SPLINE_CURVE((1.00105778586562,1.00082309557111,1.))
REPRESENTATION_ITEM('')
) ;
#238 = (
BOUNDED_CURVE()
B_SPLINE_CURVE(2,(#16163,#16164,#16165),.UNSPECIFIED.,.F.,.F.)
B_SPLINE_CURVE_WITH_KNOTS((3,3),(0.,0.0214440700661772),.UNSPECIFIED.)
CURVE()
GEOMETRIC_REPRESENTATION_ITEM()
RATIONAL_B_SPLINE_CURVE((1.,1.00082309556912,1.00105778586306))
REPRESENTATION_ITEM('')
) ;
#239 = (
BOUNDED_CURVE()
B_SPLINE_CURVE(2,(#16168,#16169,#16170),.UNSPECIFIED.,.F.,.F.)
B_SPLINE_CURVE_WITH_KNOTS((3,3),(0.0385503582641919,0.0599944283303571),
 .UNSPECIFIED.)
CURVE()
GEOMETRIC_REPRESENTATION_ITEM()
RATIONAL_B_SPLINE_CURVE((1.00105778586425,1.00082309557004,1.))
REPRESENTATION_ITEM('')
) ;
#240 = (
BOUNDED_CURVE()
B_SPLINE_CURVE(2,(#16177,#16178,#16179),.UNSPECIFIED.,.F.,.F.)
B_SPLINE_CURVE_WITH_KNOTS((3,3),(0.,0.02144407006609),.UNSPECIFIED.)
CURVE()
GEOMETRIC_REPRESENTATION_ITEM()
RATIONAL_B_SPLINE_CURVE((1.,1.0008230955718,1.00105778586652))
REPRESENTATION_ITEM('')
) ;
#241 = (
BOUNDED_CURVE()
B_SPLINE_CURVE(2,(#16182,#16183,#16184),.UNSPECIFIED.,.F.,.F.)
B_SPLINE_CURVE_WITH_KNOTS((3,3),(0.0385503582642022,0.0599944283303558),
 .UNSPECIFIED.)
CURVE()
GEOMETRIC_REPRESENTATION_ITEM()
RATIONAL_B_SPLINE_CURVE((1.00105778586255,1.00082309556872,1.))
REPRESENTATION_ITEM('')
) ;
#242 = (
BOUNDED_CURVE()
B_SPLINE_CURVE(2,(#16191,#16192,#16193),.UNSPECIFIED.,.F.,.F.)
B_SPLINE_CURVE_WITH_KNOTS((3,3),(0.,0.0214440700661625),.UNSPECIFIED.)
CURVE()
GEOMETRIC_REPRESENTATION_ITEM()
RATIONAL_B_SPLINE_CURVE((1.,1.00082309557089,1.00105778586534))
REPRESENTATION_ITEM('')
) ;
#243 = (
BOUNDED_CURVE()
B_SPLINE_CURVE(2,(#16196,#16197,#16198),.UNSPECIFIED.,.F.,.F.)
B_SPLINE_CURVE_WITH_KNOTS((3,3),(0.038550358264205,0.0599944283303565),
 .UNSPECIFIED.)
CURVE()
GEOMETRIC_REPRESENTATION_ITEM()
RATIONAL_B_SPLINE_CURVE((1.00105778586624,1.00082309557159,1.))
REPRESENTATION_ITEM('')
) ;
#244 = (
BOUNDED_CURVE()
B_SPLINE_CURVE(2,(#16205,#16206,#16207),.UNSPECIFIED.,.F.,.F.)
B_SPLINE_CURVE_WITH_KNOTS((3,3),(0.,0.0214440700661342),.UNSPECIFIED.)
CURVE()
GEOMETRIC_REPRESENTATION_ITEM()
RATIONAL_B_SPLINE_CURVE((1.,1.00082309557258,1.00105778586751))
REPRESENTATION_ITEM('')
) ;
#245 = (
BOUNDED_CURVE()
B_SPLINE_CURVE(2,(#16210,#16211,#16212),.UNSPECIFIED.,.F.,.F.)
B_SPLINE_CURVE_WITH_KNOTS((3,3),(0.0385503582641691,0.0599944283303568),
 .UNSPECIFIED.)
CURVE()
GEOMETRIC_REPRESENTATION_ITEM()
RATIONAL_B_SPLINE_CURVE((1.00105778586269,1.00082309556883,1.))
REPRESENTATION_ITEM('')
) ;
#246 = (
BOUNDED_CURVE()
B_SPLINE_CURVE(2,(#16219,#16220,#16221),.UNSPECIFIED.,.F.,.F.)
B_SPLINE_CURVE_WITH_KNOTS((3,3),(0.,0.0214440700661154),.UNSPECIFIED.)
CURVE()
GEOMETRIC_REPRESENTATION_ITEM()
RATIONAL_B_SPLINE_CURVE((1.,1.00082309557543,1.00105778587117))
REPRESENTATION_ITEM('')
) ;
#247 = (
BOUNDED_CURVE()
B_SPLINE_CURVE(2,(#16224,#16225,#16226),.UNSPECIFIED.,.F.,.F.)
B_SPLINE_CURVE_WITH_KNOTS((3,3),(0.0385503582642171,0.0599944283303574),
 .UNSPECIFIED.)
CURVE()
GEOMETRIC_REPRESENTATION_ITEM()
RATIONAL_B_SPLINE_CURVE((1.00105778586904,1.00082309557377,1.))
REPRESENTATION_ITEM('')
) ;
#248 = (
BOUNDED_CURVE()
B_SPLINE_CURVE(2,(#16233,#16234,#16235),.UNSPECIFIED.,.F.,.F.)
B_SPLINE_CURVE_WITH_KNOTS((3,3),(0.,0.0214440700661167),.UNSPECIFIED.)
CURVE()
GEOMETRIC_REPRESENTATION_ITEM()
RATIONAL_B_SPLINE_CURVE((1.,1.00082309557365,1.00105778586889))
REPRESENTATION_ITEM('')
) ;
#249 = (
BOUNDED_CURVE()
B_SPLINE_CURVE(2,(#16238,#16239,#16240),.UNSPECIFIED.,.F.,.F.)
B_SPLINE_CURVE_WITH_KNOTS((3,3),(0.0385503582642811,0.0599944283303564),
 .UNSPECIFIED.)
CURVE()
GEOMETRIC_REPRESENTATION_ITEM()
RATIONAL_B_SPLINE_CURVE((1.00105778587046,1.00082309557487,1.))
REPRESENTATION_ITEM('')
) ;
#250 = (
BOUNDED_CURVE()
B_SPLINE_CURVE(2,(#16247,#16248,#16249),.UNSPECIFIED.,.F.,.F.)
B_SPLINE_CURVE_WITH_KNOTS((3,3),(0.,0.0214440700661453),.UNSPECIFIED.)
CURVE()
GEOMETRIC_REPRESENTATION_ITEM()
RATIONAL_B_SPLINE_CURVE((1.,1.00082309557136,1.00105778586595))
REPRESENTATION_ITEM('')
) ;
#251 = (
BOUNDED_CURVE()
B_SPLINE_CURVE(2,(#16252,#16253,#16254),.UNSPECIFIED.,.F.,.F.)
B_SPLINE_CURVE_WITH_KNOTS((3,3),(0.0385503582642705,0.0599944283303552),
 .UNSPECIFIED.)
CURVE()
GEOMETRIC_REPRESENTATION_ITEM()
RATIONAL_B_SPLINE_CURVE((1.00105778586715,1.0008230955723,1.))
REPRESENTATION_ITEM('')
) ;
#252 = (
BOUNDED_CURVE()
B_SPLINE_CURVE(2,(#16261,#16262,#16263),.UNSPECIFIED.,.F.,.F.)
B_SPLINE_CURVE_WITH_KNOTS((3,3),(0.,0.0214440700661215),.UNSPECIFIED.)
CURVE()
GEOMETRIC_REPRESENTATION_ITEM()
RATIONAL_B_SPLINE_CURVE((1.,1.00082309557137,1.00105778586595))
REPRESENTATION_ITEM('')
) ;
#253 = (
BOUNDED_CURVE()
B_SPLINE_CURVE(2,(#16266,#16267,#16268),.UNSPECIFIED.,.F.,.F.)
B_SPLINE_CURVE_WITH_KNOTS((3,3),(0.0385503582641931,0.0599944283303567),
 .UNSPECIFIED.)
CURVE()
GEOMETRIC_REPRESENTATION_ITEM()
RATIONAL_B_SPLINE_CURVE((1.00105778586386,1.00082309556974,1.))
REPRESENTATION_ITEM('')
) ;
#254 = (
BOUNDED_CURVE()
B_SPLINE_CURVE(2,(#16275,#16276,#16277),.UNSPECIFIED.,.F.,.F.)
B_SPLINE_CURVE_WITH_KNOTS((3,3),(0.,0.0214440700661656),.UNSPECIFIED.)
CURVE()
GEOMETRIC_REPRESENTATION_ITEM()
RATIONAL_B_SPLINE_CURVE((1.,1.00082309557042,1.00105778586474))
REPRESENTATION_ITEM('')
) ;
#255 = (
BOUNDED_CURVE()
B_SPLINE_CURVE(2,(#16280,#16281,#16282),.UNSPECIFIED.,.F.,.F.)
B_SPLINE_CURVE_WITH_KNOTS((3,3),(0.0385503582642439,0.0599944283303563),
 .UNSPECIFIED.)
CURVE()
GEOMETRIC_REPRESENTATION_ITEM()
RATIONAL_B_SPLINE_CURVE((1.00105778586994,1.00082309557447,1.))
REPRESENTATION_ITEM('')
) ;
#256 = (
BOUNDED_CURVE()
B_SPLINE_CURVE(2,(#16289,#16290,#16291),.UNSPECIFIED.,.F.,.F.)
B_SPLINE_CURVE_WITH_KNOTS((3,3),(0.,0.0214440700660658),.UNSPECIFIED.)
CURVE()
GEOMETRIC_REPRESENTATION_ITEM()
RATIONAL_B_SPLINE_CURVE((1.,1.00082309557484,1.00105778587042))
REPRESENTATION_ITEM('')
) ;
#257 = (
BOUNDED_CURVE()
B_SPLINE_CURVE(2,(#16294,#16295,#16296),.UNSPECIFIED.,.F.,.F.)
B_SPLINE_CURVE_WITH_KNOTS((3,3),(0.0385503582642125,0.0599944283303565),
 .UNSPECIFIED.)
CURVE()
GEOMETRIC_REPRESENTATION_ITEM()
RATIONAL_B_SPLINE_CURVE((1.00105778586599,1.0008230955714,1.))
REPRESENTATION_ITEM('')
) ;
#258 = (
BOUNDED_CURVE()
B_SPLINE_CURVE(2,(#16303,#16304,#16305),.UNSPECIFIED.,.F.,.F.)
B_SPLINE_CURVE_WITH_KNOTS((3,3),(0.,0.0214440700661045),.UNSPECIFIED.)
CURVE()
GEOMETRIC_REPRESENTATION_ITEM()
RATIONAL_B_SPLINE_CURVE((1.,1.00082309557375,1.00105778586901))
REPRESENTATION_ITEM('')
) ;
#259 = (
BOUNDED_CURVE()
B_SPLINE_CURVE(2,(#16308,#16309,#16310),.UNSPECIFIED.,.F.,.F.)
B_SPLINE_CURVE_WITH_KNOTS((3,3),(0.0385503582642445,0.0599944283303561),
 .UNSPECIFIED.)
CURVE()
GEOMETRIC_REPRESENTATION_ITEM()
RATIONAL_B_SPLINE_CURVE((1.00105778586579,1.00082309557124,1.))
REPRESENTATION_ITEM('')
) ;
#260 = (
BOUNDED_CURVE()
B_SPLINE_CURVE(2,(#16317,#16318,#16319),.UNSPECIFIED.,.F.,.F.)
B_SPLINE_CURVE_WITH_KNOTS((3,3),(0.,0.021444070066132),.UNSPECIFIED.)
CURVE()
GEOMETRIC_REPRESENTATION_ITEM()
RATIONAL_B_SPLINE_CURVE((1.,1.00082309557227,1.00105778586711))
REPRESENTATION_ITEM('')
) ;
#261 = (
BOUNDED_CURVE()
B_SPLINE_CURVE(2,(#16322,#16323,#16324),.UNSPECIFIED.,.F.,.F.)
B_SPLINE_CURVE_WITH_KNOTS((3,3),(0.03855035826422,0.0599944283303558),
 .UNSPECIFIED.)
CURVE()
GEOMETRIC_REPRESENTATION_ITEM()
RATIONAL_B_SPLINE_CURVE((1.00105778586627,1.00082309557161,1.))
REPRESENTATION_ITEM('')
) ;
#262 = (
BOUNDED_CURVE()
B_SPLINE_CURVE(2,(#16331,#16332,#16333),.UNSPECIFIED.,.F.,.F.)
B_SPLINE_CURVE_WITH_KNOTS((3,3),(0.,0.0214440700661134),.UNSPECIFIED.)
CURVE()
GEOMETRIC_REPRESENTATION_ITEM()
RATIONAL_B_SPLINE_CURVE((1.,1.00082309557282,1.00105778586782))
REPRESENTATION_ITEM('')
) ;
#263 = (
BOUNDED_CURVE()
B_SPLINE_CURVE(2,(#16336,#16337,#16338),.UNSPECIFIED.,.F.,.F.)
B_SPLINE_CURVE_WITH_KNOTS((3,3),(0.0385503582642076,0.0599944283303568),
 .UNSPECIFIED.)
CURVE()
GEOMETRIC_REPRESENTATION_ITEM()
RATIONAL_B_SPLINE_CURVE((1.00105778586756,1.00082309557262,1.))
REPRESENTATION_ITEM('')
) ;
#264 = (
BOUNDED_CURVE()
B_SPLINE_CURVE(2,(#16345,#16346,#16347),.UNSPECIFIED.,.F.,.F.)
B_SPLINE_CURVE_WITH_KNOTS((3,3),(0.,0.0214440700660783),.UNSPECIFIED.)
CURVE()
GEOMETRIC_REPRESENTATION_ITEM()
RATIONAL_B_SPLINE_CURVE((1.,1.00082309557531,1.00105778587102))
REPRESENTATION_ITEM('')
) ;
#265 = (
BOUNDED_CURVE()
B_SPLINE_CURVE(2,(#16350,#16351,#16352),.UNSPECIFIED.,.F.,.F.)
B_SPLINE_CURVE_WITH_KNOTS((3,3),(0.0385503582642354,0.0599944283303562),
 .UNSPECIFIED.)
CURVE()
GEOMETRIC_REPRESENTATION_ITEM()
RATIONAL_B_SPLINE_CURVE((1.0010577858655,1.00082309557101,1.))
REPRESENTATION_ITEM('')
) ;
#266 = (
BOUNDED_CURVE()
B_SPLINE_CURVE(2,(#16359,#16360,#16361),.UNSPECIFIED.,.F.,.F.)
B_SPLINE_CURVE_WITH_KNOTS((3,3),(0.,0.021444070066152),.UNSPECIFIED.)
CURVE()
GEOMETRIC_REPRESENTATION_ITEM()
RATIONAL_B_SPLINE_CURVE((1.,1.00082309556975,1.00105778586387))
REPRESENTATION_ITEM('')
) ;
#267 = (
BOUNDED_CURVE()
B_SPLINE_CURVE(2,(#16364,#16365,#16366),.UNSPECIFIED.,.F.,.F.)
B_SPLINE_CURVE_WITH_KNOTS((3,3),(0.0385503582642177,0.0599944283303568),
 .UNSPECIFIED.)
CURVE()
GEOMETRIC_REPRESENTATION_ITEM()
RATIONAL_B_SPLINE_CURVE((1.00105778586644,1.00082309557175,1.))
REPRESENTATION_ITEM('')
) ;
#268 = (
BOUNDED_CURVE()
B_SPLINE_CURVE(2,(#16373,#16374,#16375),.UNSPECIFIED.,.F.,.F.)
B_SPLINE_CURVE_WITH_KNOTS((3,3),(0.,0.0214440700661323),.UNSPECIFIED.)
CURVE()
GEOMETRIC_REPRESENTATION_ITEM()
RATIONAL_B_SPLINE_CURVE((1.,1.00082309557161,1.00105778586626))
REPRESENTATION_ITEM('')
) ;
#269 = (
BOUNDED_CURVE()
B_SPLINE_CURVE(2,(#16378,#16379,#16380),.UNSPECIFIED.,.F.,.F.)
B_SPLINE_CURVE_WITH_KNOTS((3,3),(0.0385503582642313,0.0599944283303566),
 .UNSPECIFIED.)
CURVE()
GEOMETRIC_REPRESENTATION_ITEM()
RATIONAL_B_SPLINE_CURVE((1.00105778586689,1.0008230955721,1.))
REPRESENTATION_ITEM('')
) ;
#270 = (
BOUNDED_CURVE()
B_SPLINE_CURVE(2,(#16387,#16388,#16389),.UNSPECIFIED.,.F.,.F.)
B_SPLINE_CURVE_WITH_KNOTS((3,3),(0.,0.0214440700661231),.UNSPECIFIED.)
CURVE()
GEOMETRIC_REPRESENTATION_ITEM()
RATIONAL_B_SPLINE_CURVE((1.,1.00082309557192,1.00105778586666))
REPRESENTATION_ITEM('')
) ;
#271 = (
BOUNDED_CURVE()
B_SPLINE_CURVE(2,(#16392,#16393,#16394),.UNSPECIFIED.,.F.,.F.)
B_SPLINE_CURVE_WITH_KNOTS((3,3),(0.0385503582642438,0.0599944283303561),
 .UNSPECIFIED.)
CURVE()
GEOMETRIC_REPRESENTATION_ITEM()
RATIONAL_B_SPLINE_CURVE((1.00105778586773,1.00082309557275,1.))
REPRESENTATION_ITEM('')
) ;
#272 = (
BOUNDED_CURVE()
B_SPLINE_CURVE(2,(#16401,#16402,#16403),.UNSPECIFIED.,.F.,.F.)
B_SPLINE_CURVE_WITH_KNOTS((3,3),(0.,0.0214440700661489),.UNSPECIFIED.)
CURVE()
GEOMETRIC_REPRESENTATION_ITEM()
RATIONAL_B_SPLINE_CURVE((1.,1.00082309557108,1.00105778586558))
REPRESENTATION_ITEM('')
) ;
#273 = (
BOUNDED_CURVE()
B_SPLINE_CURVE(2,(#16406,#16407,#16408),.UNSPECIFIED.,.F.,.F.)
B_SPLINE_CURVE_WITH_KNOTS((3,3),(0.0385503582642491,0.0599944283303561),
 .UNSPECIFIED.)
CURVE()
GEOMETRIC_REPRESENTATION_ITEM()
RATIONAL_B_SPLINE_CURVE((1.00105778586862,1.00082309557344,1.))
REPRESENTATION_ITEM('')
) ;
#274 = (
BOUNDED_CURVE()
B_SPLINE_CURVE(2,(#16415,#16416,#16417),.UNSPECIFIED.,.F.,.F.)
B_SPLINE_CURVE_WITH_KNOTS((3,3),(0.,0.0214440700660912),.UNSPECIFIED.)
CURVE()
GEOMETRIC_REPRESENTATION_ITEM()
RATIONAL_B_SPLINE_CURVE((1.,1.00082309557531,1.00105778587103))
REPRESENTATION_ITEM('')
) ;
#275 = (
BOUNDED_CURVE()
B_SPLINE_CURVE(2,(#16420,#16421,#16422),.UNSPECIFIED.,.F.,.F.)
B_SPLINE_CURVE_WITH_KNOTS((3,3),(0.0385503582642475,0.0599944283303563),
 .UNSPECIFIED.)
CURVE()
GEOMETRIC_REPRESENTATION_ITEM()
RATIONAL_B_SPLINE_CURVE((1.0010577858671,1.00082309557226,1.))
REPRESENTATION_ITEM('')
) ;
#276 = (
BOUNDED_CURVE()
B_SPLINE_CURVE(2,(#16429,#16430,#16431),.UNSPECIFIED.,.F.,.F.)
B_SPLINE_CURVE_WITH_KNOTS((3,3),(0.,0.0214440700661173),.UNSPECIFIED.)
CURVE()
GEOMETRIC_REPRESENTATION_ITEM()
RATIONAL_B_SPLINE_CURVE((1.,1.00082309557298,1.00105778586803))
REPRESENTATION_ITEM('')
) ;
#277 = (
BOUNDED_CURVE()
B_SPLINE_CURVE(2,(#16434,#16435,#16436),.UNSPECIFIED.,.F.,.F.)
B_SPLINE_CURVE_WITH_KNOTS((3,3),(0.0385503582641958,0.0599944283303564),
 .UNSPECIFIED.)
CURVE()
GEOMETRIC_REPRESENTATION_ITEM()
RATIONAL_B_SPLINE_CURVE((1.00105778586416,1.00082309556997,1.))
REPRESENTATION_ITEM('')
) ;
#278 = (
BOUNDED_CURVE()
B_SPLINE_CURVE(2,(#16443,#16444,#16445),.UNSPECIFIED.,.F.,.F.)
B_SPLINE_CURVE_WITH_KNOTS((3,3),(0.,0.0214440700660895),.UNSPECIFIED.)
CURVE()
GEOMETRIC_REPRESENTATION_ITEM()
RATIONAL_B_SPLINE_CURVE((1.,1.00082309557376,1.00105778586903))
REPRESENTATION_ITEM('')
) ;
#279 = (
BOUNDED_CURVE()
B_SPLINE_CURVE(2,(#16448,#16449,#16450),.UNSPECIFIED.,.F.,.F.)
B_SPLINE_CURVE_WITH_KNOTS((3,3),(0.0385503582642543,0.0599944283303558),
 .UNSPECIFIED.)
CURVE()
GEOMETRIC_REPRESENTATION_ITEM()
RATIONAL_B_SPLINE_CURVE((1.00105778586867,1.00082309557348,1.))
REPRESENTATION_ITEM('')
) ;
#280 = (
BOUNDED_CURVE()
B_SPLINE_CURVE(2,(#16457,#16458,#16459),.UNSPECIFIED.,.F.,.F.)
B_SPLINE_CURVE_WITH_KNOTS((3,3),(0.,0.0214440700661381),.UNSPECIFIED.)
CURVE()
GEOMETRIC_REPRESENTATION_ITEM()
RATIONAL_B_SPLINE_CURVE((1.,1.00082309557261,1.00105778586756))
REPRESENTATION_ITEM('')
) ;
#281 = (
BOUNDED_CURVE()
B_SPLINE_CURVE(2,(#16462,#16463,#16464),.UNSPECIFIED.,.F.,.F.)
B_SPLINE_CURVE_WITH_KNOTS((3,3),(0.0385503582642087,0.0599944283303561),
 .UNSPECIFIED.)
CURVE()
GEOMETRIC_REPRESENTATION_ITEM()
RATIONAL_B_SPLINE_CURVE((1.00105778586395,1.0008230955698,1.))
REPRESENTATION_ITEM('')
) ;
#282 = (
BOUNDED_CURVE()
B_SPLINE_CURVE(2,(#16471,#16472,#16473),.UNSPECIFIED.,.F.,.F.)
B_SPLINE_CURVE_WITH_KNOTS((3,3),(0.,0.0214440700661082),.UNSPECIFIED.)
CURVE()
GEOMETRIC_REPRESENTATION_ITEM()
RATIONAL_B_SPLINE_CURVE((1.,1.00082309557413,1.00105778586951))
REPRESENTATION_ITEM('')
) ;
#283 = (
BOUNDED_CURVE()
B_SPLINE_CURVE(2,(#16476,#16477,#16478),.UNSPECIFIED.,.F.,.F.)
B_SPLINE_CURVE_WITH_KNOTS((3,3),(0.0385503582642435,0.0599944283303565),
 .UNSPECIFIED.)
CURVE()
GEOMETRIC_REPRESENTATION_ITEM()
RATIONAL_B_SPLINE_CURVE((1.00105778586698,1.00082309557217,1.))
REPRESENTATION_ITEM('')
) ;
#284 = (
BOUNDED_CURVE()
B_SPLINE_CURVE(2,(#16485,#16486,#16487),.UNSPECIFIED.,.F.,.F.)
B_SPLINE_CURVE_WITH_KNOTS((3,3),(0.,0.0214440700661165),.UNSPECIFIED.)
CURVE()
GEOMETRIC_REPRESENTATION_ITEM()
RATIONAL_B_SPLINE_CURVE((1.,1.00082309557299,1.00105778586805))
REPRESENTATION_ITEM('')
) ;
#285 = (
BOUNDED_CURVE()
B_SPLINE_CURVE(2,(#16490,#16491,#16492),.UNSPECIFIED.,.F.,.F.)
B_SPLINE_CURVE_WITH_KNOTS((3,3),(0.0385503582642354,0.0599944283303561),
 .UNSPECIFIED.)
CURVE()
GEOMETRIC_REPRESENTATION_ITEM()
RATIONAL_B_SPLINE_CURVE((1.00105778586729,1.00082309557241,1.))
REPRESENTATION_ITEM('')
) ;
#286 = (
BOUNDED_CURVE()
B_SPLINE_CURVE(2,(#16499,#16500,#16501),.UNSPECIFIED.,.F.,.F.)
B_SPLINE_CURVE_WITH_KNOTS((3,3),(0.,0.0214440700661208),.UNSPECIFIED.)
CURVE()
GEOMETRIC_REPRESENTATION_ITEM()
RATIONAL_B_SPLINE_CURVE((1.,1.00082309557164,1.0010577858663))
REPRESENTATION_ITEM('')
) ;
#287 = (
BOUNDED_CURVE()
B_SPLINE_CURVE(2,(#16504,#16505,#16506),.UNSPECIFIED.,.F.,.F.)
B_SPLINE_CURVE_WITH_KNOTS((3,3),(0.0385503582642138,0.0599944283303558),
 .UNSPECIFIED.)
CURVE()
GEOMETRIC_REPRESENTATION_ITEM()
RATIONAL_B_SPLINE_CURVE((1.0010577858656,1.00082309557109,1.))
REPRESENTATION_ITEM('')
) ;
#288 = (
BOUNDED_CURVE()
B_SPLINE_CURVE(2,(#16513,#16514,#16515),.UNSPECIFIED.,.F.,.F.)
B_SPLINE_CURVE_WITH_KNOTS((3,3),(0.,0.0214440700661239),.UNSPECIFIED.)
CURVE()
GEOMETRIC_REPRESENTATION_ITEM()
RATIONAL_B_SPLINE_CURVE((1.,1.00082309557102,1.0010577858655))
REPRESENTATION_ITEM('')
) ;
#289 = (
BOUNDED_CURVE()
B_SPLINE_CURVE(2,(#16518,#16519,#16520),.UNSPECIFIED.,.F.,.F.)
B_SPLINE_CURVE_WITH_KNOTS((3,3),(0.0385503582643101,0.0599944283303554),
 .UNSPECIFIED.)
CURVE()
GEOMETRIC_REPRESENTATION_ITEM()
RATIONAL_B_SPLINE_CURVE((1.00105778587441,1.00082309557795,1.))
REPRESENTATION_ITEM('')
) ;
#290 = (
BOUNDED_CURVE()
B_SPLINE_CURVE(2,(#16527,#16528,#16529),.UNSPECIFIED.,.F.,.F.)
B_SPLINE_CURVE_WITH_KNOTS((3,3),(0.,0.021444070066082),.UNSPECIFIED.)
CURVE()
GEOMETRIC_REPRESENTATION_ITEM()
RATIONAL_B_SPLINE_CURVE((1.,1.0008230955747,1.00105778587023))
REPRESENTATION_ITEM('')
) ;
#291 = (
BOUNDED_CURVE()
B_SPLINE_CURVE(2,(#16532,#16533,#16534),.UNSPECIFIED.,.F.,.F.)
B_SPLINE_CURVE_WITH_KNOTS((3,3),(0.0385503582643354,0.0599944283303546),
 .UNSPECIFIED.)
CURVE()
GEOMETRIC_REPRESENTATION_ITEM()
RATIONAL_B_SPLINE_CURVE((1.00105778587483,1.00082309557827,1.))
REPRESENTATION_ITEM('')
) ;
#292 = (
BOUNDED_CURVE()
B_SPLINE_CURVE(2,(#16541,#16542,#16543),.UNSPECIFIED.,.F.,.F.)
B_SPLINE_CURVE_WITH_KNOTS((3,3),(0.,0.0214440700660534),.UNSPECIFIED.)
CURVE()
GEOMETRIC_REPRESENTATION_ITEM()
RATIONAL_B_SPLINE_CURVE((1.,1.0008230955765,1.00105778587255))
REPRESENTATION_ITEM('')
) ;
#293 = (
BOUNDED_CURVE()
B_SPLINE_CURVE(2,(#16546,#16547,#16548),.UNSPECIFIED.,.F.,.F.)
B_SPLINE_CURVE_WITH_KNOTS((3,3),(0.038550358264337,0.0599944283303554),
 .UNSPECIFIED.)
CURVE()
GEOMETRIC_REPRESENTATION_ITEM()
RATIONAL_B_SPLINE_CURVE((1.00105778587529,1.00082309557863,1.))
REPRESENTATION_ITEM('')
) ;
#294 = (
BOUNDED_CURVE()
B_SPLINE_CURVE(2,(#16555,#16556,#16557),.UNSPECIFIED.,.F.,.F.)
B_SPLINE_CURVE_WITH_KNOTS((3,3),(0.,0.0214440700660699),.UNSPECIFIED.)
CURVE()
GEOMETRIC_REPRESENTATION_ITEM()
RATIONAL_B_SPLINE_CURVE((1.,1.00082309557688,1.00105778587304))
REPRESENTATION_ITEM('')
) ;
#295 = (
BOUNDED_CURVE()
B_SPLINE_CURVE(2,(#16560,#16561,#16562),.UNSPECIFIED.,.F.,.F.)
B_SPLINE_CURVE_WITH_KNOTS((3,3),(0.0385503582642283,0.0599944283303555),
 .UNSPECIFIED.)
CURVE()
GEOMETRIC_REPRESENTATION_ITEM()
RATIONAL_B_SPLINE_CURVE((1.00105778586715,1.0008230955723,1.))
REPRESENTATION_ITEM('')
) ;
#296 = (
BOUNDED_CURVE()
B_SPLINE_CURVE(2,(#16569,#16570,#16571),.UNSPECIFIED.,.F.,.F.)
B_SPLINE_CURVE_WITH_KNOTS((3,3),(0.,0.0214440700660926),.UNSPECIFIED.)
CURVE()
GEOMETRIC_REPRESENTATION_ITEM()
RATIONAL_B_SPLINE_CURVE((1.,1.00082309557397,1.0010577858693))
REPRESENTATION_ITEM('')
) ;
#297 = (
BOUNDED_CURVE()
B_SPLINE_CURVE(2,(#16574,#16575,#16576),.UNSPECIFIED.,.F.,.F.)
B_SPLINE_CURVE_WITH_KNOTS((3,3),(0.0385503582642555,0.0599944283303555),
 .UNSPECIFIED.)
CURVE()
GEOMETRIC_REPRESENTATION_ITEM()
RATIONAL_B_SPLINE_CURVE((1.00105778587096,1.00082309557526,1.))
REPRESENTATION_ITEM('')
) ;
#298 = (
BOUNDED_CURVE()
B_SPLINE_CURVE(2,(#16583,#16584,#16585),.UNSPECIFIED.,.F.,.F.)
B_SPLINE_CURVE_WITH_KNOTS((3,3),(0.,0.0214440700660555),.UNSPECIFIED.)
CURVE()
GEOMETRIC_REPRESENTATION_ITEM()
RATIONAL_B_SPLINE_CURVE((1.,1.00082309557703,1.00105778587323))
REPRESENTATION_ITEM('')
) ;
#299 = (
BOUNDED_CURVE()
B_SPLINE_CURVE(2,(#16588,#16589,#16590),.UNSPECIFIED.,.F.,.F.)
B_SPLINE_CURVE_WITH_KNOTS((3,3),(0.0385503582642982,0.059994428330355),
 .UNSPECIFIED.)
CURVE()
GEOMETRIC_REPRESENTATION_ITEM()
RATIONAL_B_SPLINE_CURVE((1.00105778587101,1.0008230955753,1.))
REPRESENTATION_ITEM('')
) ;
#300 = (
BOUNDED_CURVE()
B_SPLINE_CURVE(2,(#16597,#16598,#16599),.UNSPECIFIED.,.F.,.F.)
B_SPLINE_CURVE_WITH_KNOTS((3,3),(0.,0.0214440700660737),.UNSPECIFIED.)
CURVE()
GEOMETRIC_REPRESENTATION_ITEM()
RATIONAL_B_SPLINE_CURVE((1.,1.00082309557534,1.00105778587106))
REPRESENTATION_ITEM('')
) ;
#301 = (
BOUNDED_CURVE()
B_SPLINE_CURVE(2,(#16602,#16603,#16604),.UNSPECIFIED.,.F.,.F.)
B_SPLINE_CURVE_WITH_KNOTS((3,3),(0.0385503582642702,0.0599944283303555),
 .UNSPECIFIED.)
CURVE()
GEOMETRIC_REPRESENTATION_ITEM()
RATIONAL_B_SPLINE_CURVE((1.00105778587074,1.00082309557509,1.))
REPRESENTATION_ITEM('')
) ;
#302 = (
BOUNDED_CURVE()
B_SPLINE_CURVE(2,(#16611,#16612,#16613),.UNSPECIFIED.,.F.,.F.)
B_SPLINE_CURVE_WITH_KNOTS((3,3),(0.,0.0214440700660954),.UNSPECIFIED.)
CURVE()
GEOMETRIC_REPRESENTATION_ITEM()
RATIONAL_B_SPLINE_CURVE((1.,1.00082309557337,1.00105778586853))
REPRESENTATION_ITEM('')
) ;
#303 = (
BOUNDED_CURVE()
B_SPLINE_CURVE(2,(#16626,#16627,#16628),.UNSPECIFIED.,.F.,.F.)
B_SPLINE_CURVE_WITH_KNOTS((3,3),(0.,0.0128119220385747),.UNSPECIFIED.)
CURVE()
GEOMETRIC_REPRESENTATION_ITEM()
RATIONAL_B_SPLINE_CURVE((1.,1.00225826788916,1.0035731078451))
REPRESENTATION_ITEM('')
) ;
#304 = (
BOUNDED_CURVE()
B_SPLINE_CURVE(2,(#16632,#16633,#16634),.UNSPECIFIED.,.F.,.F.)
B_SPLINE_CURVE_WITH_KNOTS((3,3),(0.0485234510605496,0.0613353730991217),
 .UNSPECIFIED.)
CURVE()
GEOMETRIC_REPRESENTATION_ITEM()
RATIONAL_B_SPLINE_CURVE((1.00357310784516,1.0022582678892,1.))
REPRESENTATION_ITEM('')
) ;
#305 = (
BOUNDED_CURVE()
B_SPLINE_CURVE(2,(#16636,#16637,#16638),.UNSPECIFIED.,.F.,.F.)
B_SPLINE_CURVE_WITH_KNOTS((3,3),(0.,0.0128119217509423),.UNSPECIFIED.)
CURVE()
GEOMETRIC_REPRESENTATION_ITEM()
RATIONAL_B_SPLINE_CURVE((1.,1.00225826778645,1.00357310769076))
REPRESENTATION_ITEM('')
) ;
#306 = (
BOUNDED_CURVE()
B_SPLINE_CURVE(2,(#16642,#16643,#16644),.UNSPECIFIED.,.F.,.F.)
B_SPLINE_CURVE_WITH_KNOTS((3,3),(0.0485234554560875,0.0613353722533859),
 .UNSPECIFIED.)
CURVE()
GEOMETRIC_REPRESENTATION_ITEM()
RATIONAL_B_SPLINE_CURVE((1.00357310667489,1.00225826691386,1.))
REPRESENTATION_ITEM('')
) ;
#307 = (
BOUNDED_CURVE()
B_SPLINE_CURVE(2,(#16646,#16647,#16648),.UNSPECIFIED.,.F.,.F.)
B_SPLINE_CURVE_WITH_KNOTS((3,3),(0.,0.0128119162220165),.UNSPECIFIED.)
CURVE()
GEOMETRIC_REPRESENTATION_ITEM()
RATIONAL_B_SPLINE_CURVE((1.,1.00225826670891,1.00357310636695))
REPRESENTATION_ITEM('')
) ;
#308 = (
BOUNDED_CURVE()
B_SPLINE_CURVE(2,(#16652,#16653,#16654),.UNSPECIFIED.,.F.,.F.)
B_SPLINE_CURVE_WITH_KNOTS((3,3),(0.048523459293524,0.0613353705619148),
 .UNSPECIFIED.)
CURVE()
GEOMETRIC_REPRESENTATION_ITEM()
RATIONAL_B_SPLINE_CURVE((1.00357310535024,1.00225826583579,1.))
REPRESENTATION_ITEM('')
) ;
#309 = (
BOUNDED_CURVE()
B_SPLINE_CURVE(2,(#16656,#16657,#16658),.UNSPECIFIED.,.F.,.F.)
B_SPLINE_CURVE_WITH_KNOTS((3,3),(0.,0.0128119109807577),.UNSPECIFIED.)
CURVE()
GEOMETRIC_REPRESENTATION_ITEM()
RATIONAL_B_SPLINE_CURVE((1.,1.002258265733,1.00357310519577))
REPRESENTATION_ITEM('')
) ;
#310 = (
BOUNDED_CURVE()
B_SPLINE_CURVE(2,(#16662,#16663,#16664),.UNSPECIFIED.,.F.,.F.)
B_SPLINE_CURVE_WITH_KNOTS((3,3),(0.0485234587354268,0.0613353697161783),
 .UNSPECIFIED.)
CURVE()
GEOMETRIC_REPRESENTATION_ITEM()
RATIONAL_B_SPLINE_CURVE((1.00357310519621,1.00225826573327,1.))
REPRESENTATION_ITEM('')
) ;
#311 = (
BOUNDED_CURVE()
B_SPLINE_CURVE(2,(#16666,#16667,#16668),.UNSPECIFIED.,.F.,.F.)
B_SPLINE_CURVE_WITH_KNOTS((3,3),(0.,0.0128119112683924),.UNSPECIFIED.)
CURVE()
GEOMETRIC_REPRESENTATION_ITEM()
RATIONAL_B_SPLINE_CURVE((1.,1.00225826583572,1.00357310535012))
REPRESENTATION_ITEM('')
) ;
#312 = (
BOUNDED_CURVE()
B_SPLINE_CURVE(2,(#16672,#16673,#16674),.UNSPECIFIED.,.F.,.F.)
B_SPLINE_CURVE_WITH_KNOTS((3,3),(0.0485234543398934,0.0613353705619145),
 .UNSPECIFIED.)
CURVE()
GEOMETRIC_REPRESENTATION_ITEM()
RATIONAL_B_SPLINE_CURVE((1.00357310636678,1.0022582667088,1.))
REPRESENTATION_ITEM('')
) ;
#313 = (
BOUNDED_CURVE()
B_SPLINE_CURVE(2,(#16677,#16678,#16679),.UNSPECIFIED.,.F.,.F.)
B_SPLINE_CURVE_WITH_KNOTS((3,3),(0.,0.0128119167973088),.UNSPECIFIED.)
CURVE()
GEOMETRIC_REPRESENTATION_ITEM()
RATIONAL_B_SPLINE_CURVE((1.,1.00225826691344,1.00357310667422))
REPRESENTATION_ITEM('')
) ;
#314 = (
BOUNDED_CURVE()
B_SPLINE_CURVE(2,(#16682,#16683,#16684),.UNSPECIFIED.,.F.,.F.)
B_SPLINE_CURVE_WITH_KNOTS((3,3),(0.0485234505024517,0.0613353722533853),
 .UNSPECIFIED.)
CURVE()
GEOMETRIC_REPRESENTATION_ITEM()
RATIONAL_B_SPLINE_CURVE((1.00357310769125,1.00225826778676,1.))
REPRESENTATION_ITEM('')
) ;
#315 = SPHERICAL_SURFACE('',#8594,1.5875) ;
#316 = TOROIDAL_SURFACE('',#8446,15.9,0.4) ;
#317 = TOROIDAL_SURFACE('',#8634,2.154,0.2) ;
#318 = TOROIDAL_SURFACE('',#8827,3.3,0.2) ;
#319 = ELLIPSE('',#8347,198.783549846831,15.5) ;
#320 = ELLIPSE('',#8363,16.3431626165531,15.5) ;
#321 = ELLIPSE('',#8364,16.3920609727038,15.5) ;
#322 = ELLIPSE('',#8367,16.4076100792785,15.5) ;
#323 = ELLIPSE('',#8368,16.3701261870697,15.5) ;
#324 = ELLIPSE('',#8369,177.958118605591,15.5) ;
#325 = ELLIPSE('',#8370,206.510783338566,15.5) ;
#326 = ELLIPSE('',#8377,16.3431623815015,15.5) ;
#327 = ELLIPSE('',#8378,16.3920609727038,15.5) ;
#328 = ELLIPSE('',#8381,16.4076104906839,15.5) ;
#329 = ELLIPSE('',#8382,16.3701257903539,15.5) ;
#330 = B_SPLINE_SURFACE_WITH_KNOTS('',2,1,((#11224,#11225),(#11226,#11227),
(#11228,#11229)),.UNSPECIFIED.,.F.,.F.,.F.,(3,3),(2,2),(0.,1.),(0.,0.0650000000000004),
 .UNSPECIFIED.) ;
#331 = B_SPLINE_SURFACE_WITH_KNOTS('',2,1,((#11249,#11250),(#11251,#11252),
(#11253,#11254)),.UNSPECIFIED.,.F.,.F.,.F.,(3,3),(2,2),(0.,1.),(0.,0.0650000000000004),
 .UNSPECIFIED.) ;
#332 = B_SPLINE_SURFACE_WITH_KNOTS('',2,1,((#11271,#11272),(#11273,#11274),
(#11275,#11276)),.UNSPECIFIED.,.F.,.F.,.F.,(3,3),(2,2),(0.,1.),(0.,0.0650000000000004),
 .UNSPECIFIED.) ;
#333 = B_SPLINE_SURFACE_WITH_KNOTS('',2,1,((#11293,#11294),(#11295,#11296),
(#11297,#11298)),.UNSPECIFIED.,.F.,.F.,.F.,(3,3),(2,2),(0.,1.),(0.,0.0650000000000004),
 .UNSPECIFIED.) ;
#334 = B_SPLINE_SURFACE_WITH_KNOTS('',2,1,((#11315,#11316),(#11317,#11318),
(#11319,#11320)),.UNSPECIFIED.,.F.,.F.,.F.,(3,3),(2,2),(0.,1.),(0.,0.0650000000000004),
 .UNSPECIFIED.) ;
#335 = B_SPLINE_SURFACE_WITH_KNOTS('',2,1,((#11340,#11341),(#11342,#11343),
(#11344,#11345)),.UNSPECIFIED.,.F.,.F.,.F.,(3,3),(2,2),(0.,1.),(0.,0.0650000000000004),
 .UNSPECIFIED.) ;
#336 = B_SPLINE_SURFACE_WITH_KNOTS('',2,1,((#11359,#11360),(#11361,#11362),
(#11363,#11364)),.UNSPECIFIED.,.F.,.F.,.F.,(3,3),(2,2),(0.,1.),(0.,0.0650000000000004),
 .UNSPECIFIED.) ;
#337 = B_SPLINE_SURFACE_WITH_KNOTS('',2,1,((#11378,#11379),(#11380,#11381),
(#11382,#11383)),.UNSPECIFIED.,.F.,.F.,.F.,(3,3),(2,2),(0.,1.),(0.,0.0650000000000004),
 .UNSPECIFIED.) ;
#338 = B_SPLINE_SURFACE_WITH_KNOTS('',2,1,((#11397,#11398),(#11399,#11400),
(#11401,#11402)),.UNSPECIFIED.,.F.,.F.,.F.,(3,3),(2,2),(0.,1.),(0.,0.0650000000000004),
 .UNSPECIFIED.) ;
#339 = B_SPLINE_SURFACE_WITH_KNOTS('',2,1,((#11416,#11417),(#11418,#11419),
(#11420,#11421)),.UNSPECIFIED.,.F.,.F.,.F.,(3,3),(2,2),(0.,1.),(0.,0.0650000000000004),
 .UNSPECIFIED.) ;
#340 = B_SPLINE_SURFACE_WITH_KNOTS('',2,1,((#11438,#11439),(#11440,#11441),
(#11442,#11443)),.UNSPECIFIED.,.F.,.F.,.F.,(3,3),(2,2),(0.,1.),(0.,0.0650000000000004),
 .UNSPECIFIED.) ;
#341 = B_SPLINE_SURFACE_WITH_KNOTS('',2,1,((#11456,#11457),(#11458,#11459),
(#11460,#11461)),.UNSPECIFIED.,.F.,.F.,.F.,(3,3),(2,2),(0.,1.),(0.,0.0650000000000004),
 .UNSPECIFIED.) ;
#342 = B_SPLINE_SURFACE_WITH_KNOTS('',2,1,((#11476,#11477),(#11478,#11479),
(#11480,#11481)),.UNSPECIFIED.,.F.,.F.,.F.,(3,3),(2,2),(0.,1.),(0.,0.0650000000000004),
 .UNSPECIFIED.) ;
#343 = B_SPLINE_SURFACE_WITH_KNOTS('',2,1,((#11498,#11499),(#11500,#11501),
(#11502,#11503)),.UNSPECIFIED.,.F.,.F.,.F.,(3,3),(2,2),(0.,1.),(0.,0.0650000000000004),
 .UNSPECIFIED.) ;
#344 = B_SPLINE_SURFACE_WITH_KNOTS('',2,1,((#11517,#11518),(#11519,#11520),
(#11521,#11522)),.UNSPECIFIED.,.F.,.F.,.F.,(3,3),(2,2),(0.,1.),(0.,0.0650000000000004),
 .UNSPECIFIED.) ;
#345 = B_SPLINE_SURFACE_WITH_KNOTS('',2,1,((#11536,#11537),(#11538,#11539),
(#11540,#11541)),.UNSPECIFIED.,.F.,.F.,.F.,(3,3),(2,2),(0.,1.),(0.,0.0650000000000004),
 .UNSPECIFIED.) ;
#346 = B_SPLINE_SURFACE_WITH_KNOTS('',2,1,((#11555,#11556),(#11557,#11558),
(#11559,#11560)),.UNSPECIFIED.,.F.,.F.,.F.,(3,3),(2,2),(0.,1.),(0.,0.0650000000000004),
 .UNSPECIFIED.) ;
#347 = B_SPLINE_SURFACE_WITH_KNOTS('',2,1,((#11574,#11575),(#11576,#11577),
(#11578,#11579)),.UNSPECIFIED.,.F.,.F.,.F.,(3,3),(2,2),(0.,1.),(0.,0.0650000000000004),
 .UNSPECIFIED.) ;
#348 = B_SPLINE_SURFACE_WITH_KNOTS('',2,1,((#11590,#11591),(#11592,#11593),
(#11594,#11595)),.UNSPECIFIED.,.F.,.F.,.F.,(3,3),(2,2),(0.,1.),(0.,0.0650000000000004),
 .UNSPECIFIED.) ;
#349 = B_SPLINE_SURFACE_WITH_KNOTS('',2,1,((#11609,#11610),(#11611,#11612),
(#11613,#11614)),.UNSPECIFIED.,.F.,.F.,.F.,(3,3),(2,2),(0.,1.),(0.,0.0650000000000004),
 .UNSPECIFIED.) ;
#350 = B_SPLINE_SURFACE_WITH_KNOTS('',2,1,((#11628,#11629),(#11630,#11631),
(#11632,#11633)),.UNSPECIFIED.,.F.,.F.,.F.,(3,3),(2,2),(0.,1.),(0.,0.0650000000000004),
 .UNSPECIFIED.) ;
#351 = B_SPLINE_SURFACE_WITH_KNOTS('',2,1,((#11647,#11648),(#11649,#11650),
(#11651,#11652)),.UNSPECIFIED.,.F.,.F.,.F.,(3,3),(2,2),(0.,1.),(0.,0.0650000000000004),
 .UNSPECIFIED.) ;
#352 = B_SPLINE_SURFACE_WITH_KNOTS('',2,1,((#11672,#11673),(#11674,#11675),
(#11676,#11677)),.UNSPECIFIED.,.F.,.F.,.F.,(3,3),(2,2),(0.,1.),(0.,0.0650000000000004),
 .UNSPECIFIED.) ;
#353 = B_SPLINE_SURFACE_WITH_KNOTS('',2,1,((#11691,#11692),(#11693,#11694),
(#11695,#11696)),.UNSPECIFIED.,.F.,.F.,.F.,(3,3),(2,2),(0.,1.),(0.,0.0650000000000004),
 .UNSPECIFIED.) ;
#354 = B_SPLINE_SURFACE_WITH_KNOTS('',2,1,((#11710,#11711),(#11712,#11713),
(#11714,#11715)),.UNSPECIFIED.,.F.,.F.,.F.,(3,3),(2,2),(0.,1.),(0.,0.0650000000000004),
 .UNSPECIFIED.) ;
#355 = B_SPLINE_SURFACE_WITH_KNOTS('',2,1,((#11732,#11733),(#11734,#11735),
(#11736,#11737)),.UNSPECIFIED.,.F.,.F.,.F.,(3,3),(2,2),(0.,1.),(0.,0.0650000000000004),
 .UNSPECIFIED.) ;
#356 = B_SPLINE_SURFACE_WITH_KNOTS('',2,1,((#11763,#11764),(#11765,#11766),
(#11767,#11768)),.UNSPECIFIED.,.F.,.F.,.F.,(3,3),(2,2),(0.,1.),(0.,0.0650000000000004),
 .UNSPECIFIED.) ;
#357 = B_SPLINE_SURFACE_WITH_KNOTS('',2,1,((#11780,#11781),(#11782,#11783),
(#11784,#11785)),.UNSPECIFIED.,.F.,.F.,.F.,(3,3),(2,2),(0.,1.),(0.,0.0650000000000004),
 .UNSPECIFIED.) ;
#358 = B_SPLINE_SURFACE_WITH_KNOTS('',2,1,((#11808,#11809),(#11810,#11811),
(#11812,#11813)),.UNSPECIFIED.,.F.,.F.,.F.,(3,3),(2,2),(0.,1.),(0.,0.0650000000000004),
 .UNSPECIFIED.) ;
#359 = B_SPLINE_SURFACE_WITH_KNOTS('',2,1,((#11827,#11828),(#11829,#11830),
(#11831,#11832)),.UNSPECIFIED.,.F.,.F.,.F.,(3,3),(2,2),(0.,1.),(0.,0.0650000000000004),
 .UNSPECIFIED.) ;
#360 = B_SPLINE_SURFACE_WITH_KNOTS('',2,1,((#11852,#11853),(#11854,#11855),
(#11856,#11857)),.UNSPECIFIED.,.F.,.F.,.F.,(3,3),(2,2),(0.,1.),(0.,0.0650000000000004),
 .UNSPECIFIED.) ;
#361 = B_SPLINE_SURFACE_WITH_KNOTS('',2,1,((#12604,#12605),(#12606,#12607),
(#12608,#12609)),.UNSPECIFIED.,.F.,.F.,.F.,(3,3),(2,2),(0.,1.),(0.,0.0650000000000004),
 .UNSPECIFIED.) ;
#362 = B_SPLINE_SURFACE_WITH_KNOTS('',2,1,((#12615,#12616),(#12617,#12618),
(#12619,#12620)),.UNSPECIFIED.,.F.,.F.,.F.,(3,3),(2,2),(0.,1.),(0.,0.0650000000000004),
 .UNSPECIFIED.) ;
#363 = B_SPLINE_SURFACE_WITH_KNOTS('',2,1,((#12641,#12642),(#12643,#12644),
(#12645,#12646)),.UNSPECIFIED.,.F.,.F.,.F.,(3,3),(2,2),(0.,1.),(0.,0.0650000000000004),
 .UNSPECIFIED.) ;
#364 = B_SPLINE_SURFACE_WITH_KNOTS('',2,1,((#12666,#12667),(#12668,#12669),
(#12670,#12671)),.UNSPECIFIED.,.F.,.F.,.F.,(3,3),(2,2),(0.,1.),(0.,0.0650000000000004),
 .UNSPECIFIED.) ;
#365 = B_SPLINE_SURFACE_WITH_KNOTS('',2,1,((#12677,#12678),(#12679,#12680),
(#12681,#12682)),.UNSPECIFIED.,.F.,.F.,.F.,(3,3),(2,2),(0.,1.),(0.,0.0650000000000004),
 .UNSPECIFIED.) ;
#366 = B_SPLINE_SURFACE_WITH_KNOTS('',2,1,((#12688,#12689),(#12690,#12691),
(#12692,#12693)),.UNSPECIFIED.,.F.,.F.,.F.,(3,3),(2,2),(0.,1.),(0.,0.0650000000000004),
 .UNSPECIFIED.) ;
#367 = B_SPLINE_SURFACE_WITH_KNOTS('',2,1,((#12699,#12700),(#12701,#12702),
(#12703,#12704)),.UNSPECIFIED.,.F.,.F.,.F.,(3,3),(2,2),(0.,1.),(0.,0.0650000000000004),
 .UNSPECIFIED.) ;
#368 = B_SPLINE_SURFACE_WITH_KNOTS('',2,1,((#12710,#12711),(#12712,#12713),
(#12714,#12715)),.UNSPECIFIED.,.F.,.F.,.F.,(3,3),(2,2),(0.,1.),(0.,0.0650000000000004),
 .UNSPECIFIED.) ;
#369 = B_SPLINE_SURFACE_WITH_KNOTS('',2,1,((#12721,#12722),(#12723,#12724),
(#12725,#12726)),.UNSPECIFIED.,.F.,.F.,.F.,(3,3),(2,2),(0.,1.),(0.,0.0650000000000004),
 .UNSPECIFIED.) ;
#370 = B_SPLINE_SURFACE_WITH_KNOTS('',2,1,((#12732,#12733),(#12734,#12735),
(#12736,#12737)),.UNSPECIFIED.,.F.,.F.,.F.,(3,3),(2,2),(0.,1.),(0.,0.0650000000000004),
 .UNSPECIFIED.) ;
#371 = B_SPLINE_SURFACE_WITH_KNOTS('',2,1,((#12743,#12744),(#12745,#12746),
(#12747,#12748)),.UNSPECIFIED.,.F.,.F.,.F.,(3,3),(2,2),(0.,1.),(0.,0.0650000000000004),
 .UNSPECIFIED.) ;
#372 = B_SPLINE_SURFACE_WITH_KNOTS('',2,1,((#12754,#12755),(#12756,#12757),
(#12758,#12759)),.UNSPECIFIED.,.F.,.F.,.F.,(3,3),(2,2),(0.,1.),(0.,0.0650000000000004),
 .UNSPECIFIED.) ;
#373 = B_SPLINE_SURFACE_WITH_KNOTS('',2,1,((#12765,#12766),(#12767,#12768),
(#12769,#12770)),.UNSPECIFIED.,.F.,.F.,.F.,(3,3),(2,2),(0.,1.),(0.,0.0650000000000004),
 .UNSPECIFIED.) ;
#374 = B_SPLINE_SURFACE_WITH_KNOTS('',2,1,((#12787,#12788),(#12789,#12790),
(#12791,#12792)),.UNSPECIFIED.,.F.,.F.,.F.,(3,3),(2,2),(0.,1.),(0.,0.0650000000000004),
 .UNSPECIFIED.) ;
#375 = B_SPLINE_SURFACE_WITH_KNOTS('',2,1,((#12800,#12801),(#12802,#12803),
(#12804,#12805)),.UNSPECIFIED.,.F.,.F.,.F.,(3,3),(2,2),(0.,1.),(0.,0.0650000000000004),
 .UNSPECIFIED.) ;
#376 = B_SPLINE_SURFACE_WITH_KNOTS('',2,1,((#12811,#12812),(#12813,#12814),
(#12815,#12816)),.UNSPECIFIED.,.F.,.F.,.F.,(3,3),(2,2),(0.,1.),(0.,0.0650000000000004),
 .UNSPECIFIED.) ;
#377 = B_SPLINE_SURFACE_WITH_KNOTS('',2,1,((#12826,#12827),(#12828,#12829),
(#12830,#12831)),.UNSPECIFIED.,.F.,.F.,.F.,(3,3),(2,2),(0.,1.),(0.,0.0650000000000004),
 .UNSPECIFIED.) ;
#378 = B_SPLINE_SURFACE_WITH_KNOTS('',2,1,((#12837,#12838),(#12839,#12840),
(#12841,#12842)),.UNSPECIFIED.,.F.,.F.,.F.,(3,3),(2,2),(0.,1.),(0.,0.0650000000000004),
 .UNSPECIFIED.) ;
#379 = B_SPLINE_SURFACE_WITH_KNOTS('',2,1,((#12848,#12849),(#12850,#12851),
(#12852,#12853)),.UNSPECIFIED.,.F.,.F.,.F.,(3,3),(2,2),(0.,1.),(0.,0.0650000000000004),
 .UNSPECIFIED.) ;
#380 = B_SPLINE_SURFACE_WITH_KNOTS('',2,1,((#12859,#12860),(#12861,#12862),
(#12863,#12864)),.UNSPECIFIED.,.F.,.F.,.F.,(3,3),(2,2),(0.,1.),(0.,0.0650000000000004),
 .UNSPECIFIED.) ;
#381 = B_SPLINE_SURFACE_WITH_KNOTS('',2,1,((#12870,#12871),(#12872,#12873),
(#12874,#12875)),.UNSPECIFIED.,.F.,.F.,.F.,(3,3),(2,2),(0.,1.),(0.,0.0650000000000004),
 .UNSPECIFIED.) ;
#382 = B_SPLINE_SURFACE_WITH_KNOTS('',2,1,((#12881,#12882),(#12883,#12884),
(#12885,#12886)),.UNSPECIFIED.,.F.,.F.,.F.,(3,3),(2,2),(0.,1.),(0.,0.0650000000000004),
 .UNSPECIFIED.) ;
#383 = B_SPLINE_SURFACE_WITH_KNOTS('',2,1,((#12892,#12893),(#12894,#12895),
(#12896,#12897)),.UNSPECIFIED.,.F.,.F.,.F.,(3,3),(2,2),(0.,1.),(0.,0.0650000000000004),
 .UNSPECIFIED.) ;
#384 = B_SPLINE_SURFACE_WITH_KNOTS('',2,1,((#12903,#12904),(#12905,#12906),
(#12907,#12908)),.UNSPECIFIED.,.F.,.F.,.F.,(3,3),(2,2),(0.,1.),(0.,0.0650000000000004),
 .UNSPECIFIED.) ;
#385 = B_SPLINE_SURFACE_WITH_KNOTS('',2,1,((#12914,#12915),(#12916,#12917),
(#12918,#12919)),.UNSPECIFIED.,.F.,.F.,.F.,(3,3),(2,2),(0.,1.),(0.,0.0650000000000004),
 .UNSPECIFIED.) ;
#386 = B_SPLINE_SURFACE_WITH_KNOTS('',2,1,((#12925,#12926),(#12927,#12928),
(#12929,#12930)),.UNSPECIFIED.,.F.,.F.,.F.,(3,3),(2,2),(0.,1.),(0.,0.0650000000000004),
 .UNSPECIFIED.) ;
#387 = B_SPLINE_SURFACE_WITH_KNOTS('',2,1,((#12936,#12937),(#12938,#12939),
(#12940,#12941)),.UNSPECIFIED.,.F.,.F.,.F.,(3,3),(2,2),(0.,1.),(0.,0.0650000000000004),
 .UNSPECIFIED.) ;
#388 = B_SPLINE_SURFACE_WITH_KNOTS('',2,1,((#12947,#12948),(#12949,#12950),
(#12951,#12952)),.UNSPECIFIED.,.F.,.F.,.F.,(3,3),(2,2),(0.,1.),(0.,0.0650000000000004),
 .UNSPECIFIED.) ;
#389 = B_SPLINE_SURFACE_WITH_KNOTS('',2,1,((#12958,#12959),(#12960,#12961),
(#12962,#12963)),.UNSPECIFIED.,.F.,.F.,.F.,(3,3),(2,2),(0.,1.),(0.,0.0650000000000004),
 .UNSPECIFIED.) ;
#390 = B_SPLINE_SURFACE_WITH_KNOTS('',2,1,((#12969,#12970),(#12971,#12972),
(#12973,#12974)),.UNSPECIFIED.,.F.,.F.,.F.,(3,3),(2,2),(0.,1.),(0.,0.0650000000000004),
 .UNSPECIFIED.) ;
#391 = B_SPLINE_SURFACE_WITH_KNOTS('',2,1,((#12980,#12981),(#12982,#12983),
(#12984,#12985)),.UNSPECIFIED.,.F.,.F.,.F.,(3,3),(2,2),(0.,1.),(0.,0.0650000000000004),
 .UNSPECIFIED.) ;
#392 = B_SPLINE_SURFACE_WITH_KNOTS('',2,1,((#12991,#12992),(#12993,#12994),
(#12995,#12996)),.UNSPECIFIED.,.F.,.F.,.F.,(3,3),(2,2),(0.,1.),(0.,0.0650000000000004),
 .UNSPECIFIED.) ;
#393 = B_SPLINE_SURFACE_WITH_KNOTS('',2,1,((#13002,#13003),(#13004,#13005),
(#13006,#13007)),.UNSPECIFIED.,.F.,.F.,.F.,(3,3),(2,2),(0.,1.),(0.,0.0650000000000004),
 .UNSPECIFIED.) ;
#394 = B_SPLINE_SURFACE_WITH_KNOTS('',2,1,((#13013,#13014),(#13015,#13016),
(#13017,#13018)),.UNSPECIFIED.,.F.,.F.,.F.,(3,3),(2,2),(0.,1.),(0.,0.0650000000000004),
 .UNSPECIFIED.) ;
#395 = B_SPLINE_SURFACE_WITH_KNOTS('',2,1,((#13024,#13025),(#13026,#13027),
(#13028,#13029)),.UNSPECIFIED.,.F.,.F.,.F.,(3,3),(2,2),(0.,1.),(0.,0.0650000000000004),
 .UNSPECIFIED.) ;
#396 = B_SPLINE_SURFACE_WITH_KNOTS('',2,1,((#13035,#13036),(#13037,#13038),
(#13039,#13040)),.UNSPECIFIED.,.F.,.F.,.F.,(3,3),(2,2),(0.,1.),(0.,0.0650000000000004),
 .UNSPECIFIED.) ;
#397 = B_SPLINE_SURFACE_WITH_KNOTS('',2,1,((#13046,#13047),(#13048,#13049),
(#13050,#13051)),.UNSPECIFIED.,.F.,.F.,.F.,(3,3),(2,2),(0.,1.),(0.,0.0650000000000004),
 .UNSPECIFIED.) ;
#398 = B_SPLINE_SURFACE_WITH_KNOTS('',2,1,((#13057,#13058),(#13059,#13060),
(#13061,#13062)),.UNSPECIFIED.,.F.,.F.,.F.,(3,3),(2,2),(0.,1.),(0.,0.0650000000000004),
 .UNSPECIFIED.) ;
#399 = B_SPLINE_SURFACE_WITH_KNOTS('',2,1,((#13068,#13069),(#13070,#13071),
(#13072,#13073)),.UNSPECIFIED.,.F.,.F.,.F.,(3,3),(2,2),(0.,1.),(0.,0.0650000000000004),
 .UNSPECIFIED.) ;
#400 = B_SPLINE_SURFACE_WITH_KNOTS('',2,1,((#13079,#13080),(#13081,#13082),
(#13083,#13084)),.UNSPECIFIED.,.F.,.F.,.F.,(3,3),(2,2),(0.,1.),(0.,0.0650000000000004),
 .UNSPECIFIED.) ;
#401 = B_SPLINE_SURFACE_WITH_KNOTS('',2,1,((#13090,#13091),(#13092,#13093),
(#13094,#13095)),.UNSPECIFIED.,.F.,.F.,.F.,(3,3),(2,2),(0.,1.),(0.,0.0650000000000004),
 .UNSPECIFIED.) ;
#402 = B_SPLINE_SURFACE_WITH_KNOTS('',2,1,((#13101,#13102),(#13103,#13104),
(#13105,#13106)),.UNSPECIFIED.,.F.,.F.,.F.,(3,3),(2,2),(0.,1.),(0.,0.0650000000000004),
 .UNSPECIFIED.) ;
#403 = B_SPLINE_SURFACE_WITH_KNOTS('',2,1,((#13112,#13113),(#13114,#13115),
(#13116,#13117)),.UNSPECIFIED.,.F.,.F.,.F.,(3,3),(2,2),(0.,1.),(0.,0.0650000000000004),
 .UNSPECIFIED.) ;
#404 = B_SPLINE_SURFACE_WITH_KNOTS('',2,1,((#13123,#13124),(#13125,#13126),
(#13127,#13128)),.UNSPECIFIED.,.F.,.F.,.F.,(3,3),(2,2),(0.,1.),(0.,0.0650000000000004),
 .UNSPECIFIED.) ;
#405 = B_SPLINE_SURFACE_WITH_KNOTS('',2,1,((#13134,#13135),(#13136,#13137),
(#13138,#13139)),.UNSPECIFIED.,.F.,.F.,.F.,(3,3),(2,2),(0.,1.),(0.,0.0650000000000004),
 .UNSPECIFIED.) ;
#406 = B_SPLINE_SURFACE_WITH_KNOTS('',2,1,((#13149,#13150),(#13151,#13152),
(#13153,#13154)),.UNSPECIFIED.,.F.,.F.,.F.,(3,3),(2,2),(0.,1.),(0.,0.0650000000000004),
 .UNSPECIFIED.) ;
#407 = B_SPLINE_SURFACE_WITH_KNOTS('',2,1,((#13197,#13198),(#13199,#13200),
(#13201,#13202)),.UNSPECIFIED.,.F.,.F.,.F.,(3,3),(2,2),(0.,1.),(0.,0.0650000000000004),
 .UNSPECIFIED.) ;
#408 = B_SPLINE_SURFACE_WITH_KNOTS('',2,1,((#13208,#13209),(#13210,#13211),
(#13212,#13213)),.UNSPECIFIED.,.F.,.F.,.F.,(3,3),(2,2),(0.,1.),(0.,0.0650000000000004),
 .UNSPECIFIED.) ;
#409 = B_SPLINE_SURFACE_WITH_KNOTS('',3,3,((#13256,#13257,#13258,#13259,#13260,
#13261),(#13262,#13263,#13264,#13265,#13266,#13267),(#13268,#13269,#13270,
#13271,#13272,#13273),(#13274,#13275,#13276,#13277,#13278,#13279)),
 .UNSPECIFIED.,.F.,.F.,.F.,(4,4),(4,1,1,4),(0.,1.),(-1.05732256406473,-0.901937192254856,
-0.746551820444979,-0.513473762730163),.UNSPECIFIED.) ;
#410 = B_SPLINE_SURFACE_WITH_KNOTS('',3,3,((#13341,#13342,#13343,#13344,#13345,
#13346),(#13347,#13348,#13349,#13350,#13351,#13352),(#13353,#13354,#13355,
#13356,#13357,#13358),(#13359,#13360,#13361,#13362,#13363,#13364)),
 .UNSPECIFIED.,.F.,.F.,.F.,(4,4),(4,1,1,4),(0.,1.),(0.513473762730164,0.746551820444979,
0.901937192254856,1.05732256406473),.UNSPECIFIED.) ;
#411 = B_SPLINE_SURFACE_WITH_KNOTS('',3,3,((#13384,#13385,#13386,#13387,#13388,
#13389),(#13390,#13391,#13392,#13393,#13394,#13395),(#13396,#13397,#13398,
#13399,#13400,#13401),(#13402,#13403,#13404,#13405,#13406,#13407)),
 .UNSPECIFIED.,.F.,.F.,.F.,(4,4),(4,1,1,4),(0.,1.),(-4.19891521765453,-4.04352984584465,
-3.88814447403477,-3.65506641631996),.UNSPECIFIED.) ;
#412 = B_SPLINE_SURFACE_WITH_KNOTS('',3,3,((#13427,#13428,#13429,#13430,#13431,
#13432),(#13433,#13434,#13435,#13436,#13437,#13438),(#13439,#13440,#13441,
#13442,#13443,#13444),(#13445,#13446,#13447,#13448,#13449,#13450)),
 .UNSPECIFIED.,.F.,.F.,.F.,(4,4),(4,1,1,4),(0.,1.),(-2.62811889085963,-2.39504083314481,
-2.23965546133494,-2.08427008952506),.UNSPECIFIED.) ;
#413 = B_SPLINE_SURFACE_WITH_KNOTS('',3,3,((#14885,#14886,#14887,#14888,#14889,
#14890,#14891,#14892,#14893,#14894,#14895,#14896,#14897,#14898,#14899,#14900,
#14901,#14902,#14903,#14904,#14905,#14906,#14907,#14908,#14909,#14910,#14911,
#14912,#14913,#14914,#14915,#14916,#14917,#14918,#14919,#14920,#14921,#14922,
#14923,#14924,#14925,#14926,#14927,#14928,#14929,#14930,#14931,#14932,#14933,
#14934,#14935,#14936,#14937,#14938,#14939,#14940,#14941,#14942,#14943,#14944,
#14945,#14946,#14947,#14948,#14949,#14950,#14951,#14952,#14953,#14954,#14955,
#14956,#14957,#14958,#14959,#14960,#14961,#14962,#14963,#14964,#14965,#14966,
#14967,#14968,#14969,#14970,#14971,#14972,#14973),(#14974,#14975,#14976,
#14977,#14978,#14979,#14980,#14981,#14982,#14983,#14984,#14985,#14986,#14987,
#14988,#14989,#14990,#14991,#14992,#14993,#14994,#14995,#14996,#14997,#14998,
#14999,#15000,#15001,#15002,#15003,#15004,#15005,#15006,#15007,#15008,#15009,
#15010,#15011,#15012,#15013,#15014,#15015,#15016,#15017,#15018,#15019,#15020,
#15021,#15022,#15023,#15024,#15025,#15026,#15027,#15028,#15029,#15030,#15031,
#15032,#15033,#15034,#15035,#15036,#15037,#15038,#15039,#15040,#15041,#15042,
#15043,#15044,#15045,#15046,#15047,#15048,#15049,#15050,#15051,#15052,#15053,
#15054,#15055,#15056,#15057,#15058,#15059,#15060,#15061,#15062),(#15063,
#15064,#15065,#15066,#15067,#15068,#15069,#15070,#15071,#15072,#15073,#15074,
#15075,#15076,#15077,#15078,#15079,#15080,#15081,#15082,#15083,#15084,#15085,
#15086,#15087,#15088,#15089,#15090,#15091,#15092,#15093,#15094,#15095,#15096,
#15097,#15098,#15099,#15100,#15101,#15102,#15103,#15104,#15105,#15106,#15107,
#15108,#15109,#15110,#15111,#15112,#15113,#15114,#15115,#15116,#15117,#15118,
#15119,#15120,#15121,#15122,#15123,#15124,#15125,#15126,#15127,#15128,#15129,
#15130,#15131,#15132,#15133,#15134,#15135,#15136,#15137,#15138,#15139,#15140,
#15141,#15142,#15143,#15144,#15145,#15146,#15147,#15148,#15149,#15150,#15151),
(#15152,#15153,#15154,#15155,#15156,#15157,#15158,#15159,#15160,#15161,
#15162,#15163,#15164,#15165,#15166,#15167,#15168,#15169,#15170,#15171,#15172,
#15173,#15174,#15175,#15176,#15177,#15178,#15179,#15180,#15181,#15182,#15183,
#15184,#15185,#15186,#15187,#15188,#15189,#15190,#15191,#15192,#15193,#15194,
#15195,#15196,#15197,#15198,#15199,#15200,#15201,#15202,#15203,#15204,#15205,
#15206,#15207,#15208,#15209,#15210,#15211,#15212,#15213,#15214,#15215,#15216,
#15217,#15218,#15219,#15220,#15221,#15222,#15223,#15224,#15225,#15226,#15227,
#15228,#15229,#15230,#15231,#15232,#15233,#15234,#15235,#15236,#15237,#15238,
#15239,#15240)),.UNSPECIFIED.,.F.,.F.,.F.,(4,4),(4,1,1,1,1,1,1,1,1,1,1,
1,1,1,1,1,1,1,1,1,1,1,1,1,1,1,1,1,1,1,1,1,1,1,1,1,1,1,1,1,1,1,1,1,1,1,1,
1,1,1,1,1,1,1,1,1,1,1,1,1,1,1,1,1,1,1,1,1,1,1,1,1,1,1,1,1,1,1,1,1,1,1,1,
1,1,1,4),(0.,0.0460148164544131),(8.31058692273963,9.30525837539851,10.2999298280574,
11.2946012807163,12.2892727333752,13.2839441860341,14.2786156386929,15.2732870913518,
16.2679585440107,17.2626299966696,18.2573014493285,19.2519729019874,20.2466443546463,
21.2413158073051,22.235987259964,23.2306587126229,24.2253301652818,25.2200016179407,
26.2146730705996,27.2093445232584,28.2040159759173,29.1986874285762,30.1933588812351,
31.188030333894,32.1827017865529,33.1773732392118,34.1720446918706,35.1667161445295,
36.1613875971884,37.1560590498473,38.1507305025062,39.1454019551651,40.1400734078239,
41.1347448604828,42.1294163131417,43.1240877658006,44.1187592184595,45.1134306711184,
46.1081021237773,47.1027735764361,48.097445029095,49.0921164817539,50.0867879344128,
51.0814593870717,52.0761308397306,53.0708022923895,54.0654737450483,55.0601451977072,
56.0548166503661,57.049488103025,58.0441595556839,59.0388310083428,60.0335024610017,
61.0281739136605,62.0228453663194,63.0175168189783,64.0121882716372,65.0068597242961,
66.001531176955,66.9962026296138,67.9908740822727,68.9855455349316,69.9802169875905,
70.9748884402494,71.9695598929083,72.9642313455672,73.958902798226,74.9535742508849,
75.9482457035438,76.9429171562027,77.9375886088616,78.9322600615205,79.9269315141794,
80.9216029668382,81.9162744194971,82.910945872156,83.9056173248149,84.9002887774738,
85.8949602301327,86.8896316827915,87.8843031354504,88.8789745881093,89.8736460407682,
90.8683174934271,91.862988946086,92.8576603987449,93.8523318514037),
 .UNSPECIFIED.) ;
#414 = B_SPLINE_SURFACE_WITH_KNOTS('',3,3,((#15446,#15447,#15448,#15449,#15450,
#15451,#15452,#15453,#15454,#15455,#15456,#15457,#15458,#15459,#15460,#15461,
#15462,#15463,#15464,#15465,#15466,#15467,#15468,#15469,#15470,#15471,#15472,
#15473,#15474,#15475,#15476,#15477,#15478,#15479,#15480,#15481,#15482,#15483,
#15484,#15485,#15486,#15487,#15488,#15489,#15490,#15491,#15492,#15493,#15494,
#15495,#15496,#15497,#15498,#15499,#15500,#15501,#15502,#15503,#15504,#15505,
#15506,#15507,#15508,#15509,#15510,#15511,#15512,#15513,#15514,#15515,#15516,
#15517,#15518,#15519,#15520,#15521,#15522,#15523,#15524,#15525,#15526,#15527,
#15528,#15529,#15530,#15531,#15532,#15533,#15534),(#15535,#15536,#15537,
#15538,#15539,#15540,#15541,#15542,#15543,#15544,#15545,#15546,#15547,#15548,
#15549,#15550,#15551,#15552,#15553,#15554,#15555,#15556,#15557,#15558,#15559,
#15560,#15561,#15562,#15563,#15564,#15565,#15566,#15567,#15568,#15569,#15570,
#15571,#15572,#15573,#15574,#15575,#15576,#15577,#15578,#15579,#15580,#15581,
#15582,#15583,#15584,#15585,#15586,#15587,#15588,#15589,#15590,#15591,#15592,
#15593,#15594,#15595,#15596,#15597,#15598,#15599,#15600,#15601,#15602,#15603,
#15604,#15605,#15606,#15607,#15608,#15609,#15610,#15611,#15612,#15613,#15614,
#15615,#15616,#15617,#15618,#15619,#15620,#15621,#15622,#15623),(#15624,
#15625,#15626,#15627,#15628,#15629,#15630,#15631,#15632,#15633,#15634,#15635,
#15636,#15637,#15638,#15639,#15640,#15641,#15642,#15643,#15644,#15645,#15646,
#15647,#15648,#15649,#15650,#15651,#15652,#15653,#15654,#15655,#15656,#15657,
#15658,#15659,#15660,#15661,#15662,#15663,#15664,#15665,#15666,#15667,#15668,
#15669,#15670,#15671,#15672,#15673,#15674,#15675,#15676,#15677,#15678,#15679,
#15680,#15681,#15682,#15683,#15684,#15685,#15686,#15687,#15688,#15689,#15690,
#15691,#15692,#15693,#15694,#15695,#15696,#15697,#15698,#15699,#15700,#15701,
#15702,#15703,#15704,#15705,#15706,#15707,#15708,#15709,#15710,#15711,#15712),
(#15713,#15714,#15715,#15716,#15717,#15718,#15719,#15720,#15721,#15722,
#15723,#15724,#15725,#15726,#15727,#15728,#15729,#15730,#15731,#15732,#15733,
#15734,#15735,#15736,#15737,#15738,#15739,#15740,#15741,#15742,#15743,#15744,
#15745,#15746,#15747,#15748,#15749,#15750,#15751,#15752,#15753,#15754,#15755,
#15756,#15757,#15758,#15759,#15760,#15761,#15762,#15763,#15764,#15765,#15766,
#15767,#15768,#15769,#15770,#15771,#15772,#15773,#15774,#15775,#15776,#15777,
#15778,#15779,#15780,#15781,#15782,#15783,#15784,#15785,#15786,#15787,#15788,
#15789,#15790,#15791,#15792,#15793,#15794,#15795,#15796,#15797,#15798,#15799,
#15800,#15801)),.UNSPECIFIED.,.F.,.F.,.F.,(4,4),(4,1,1,1,1,1,1,1,1,1,1,
1,1,1,1,1,1,1,1,1,1,1,1,1,1,1,1,1,1,1,1,1,1,1,1,1,1,1,1,1,1,1,1,1,1,1,1,
1,1,1,1,1,1,1,1,1,1,1,1,1,1,1,1,1,1,1,1,1,1,1,1,1,1,1,1,1,1,1,1,1,1,1,1,
1,1,1,4),(0.,0.0460148164544131),(11.6154215191105,12.6100929717694,13.6047644244283,
14.5994358770872,15.594107329746,16.5887787824049,17.5834502350638,18.5781216877227,
19.5727931403816,20.5674645930405,21.5621360456994,22.5568074983582,23.5514789510171,
24.546150403676,25.5408218563349,26.5354933089938,27.5301647616527,28.5248362143116,
29.5195076669704,30.5141791196293,31.5088505722882,32.5035220249471,33.498193477606,
34.4928649302649,35.4875363829238,36.4822078355826,37.4768792882415,38.4715507409004,
39.4662221935593,40.4608936462182,41.4555650988771,42.450236551536,43.4449080041948,
44.4395794568537,45.4342509095126,46.4289223621715,47.4235938148304,48.4182652674893,
49.4129367201481,50.407608172807,51.4022796254659,52.3969510781248,53.3916225307837,
54.3862939834426,55.3809654361015,56.3756368887603,57.3703083414192,58.3649797940781,
59.359651246737,60.3543226993959,61.3489941520548,62.3436656047136,63.3383370573725,
64.3330085100314,65.3276799626903,66.3223514153492,67.3170228680081,68.311694320667,
69.3063657733259,70.3010372259847,71.2957086786436,72.2903801313025,73.2850515839614,
74.2797230366203,75.2743944892792,76.2690659419381,77.2637373945969,78.2584088472558,
79.2530802999147,80.2477517525736,81.2424232052325,82.2370946578914,83.2317661105503,
84.2264375632091,85.221109015868,86.2157804685269,87.2104519211858,88.2051233738447,
89.1997948265036,90.1944662791624,91.1891377318213,92.1838091844802,93.1784806371391,
94.173152089798,95.1678235424569,96.1624949951158,97.1571664477746),
 .UNSPECIFIED.) ;
#415 = SHAPE_REPRESENTATION_RELATIONSHIP('SRR','None',#17019,#422) ;
#416 = SHAPE_REPRESENTATION_RELATIONSHIP('SRR','None',#17020,#423) ;
#417 = SHAPE_REPRESENTATION_RELATIONSHIP('SRR','None',#17021,#424) ;
#418 = SHAPE_REPRESENTATION_RELATIONSHIP('SRR','None',#17022,#425) ;
#419 = SHAPE_REPRESENTATION_RELATIONSHIP('SRR','None',#17023,#426) ;
#420 = SHAPE_REPRESENTATION_RELATIONSHIP('SRR','None',#17024,#427) ;
#421 = SHAPE_REPRESENTATION_RELATIONSHIP('SRR','None',#17025,#428) ;
#422 = ADVANCED_BREP_SHAPE_REPRESENTATION('',(#436),#16935) ;
#423 = ADVANCED_BREP_SHAPE_REPRESENTATION('',(#437),#16936) ;
#424 = ADVANCED_BREP_SHAPE_REPRESENTATION('',(#438),#16937) ;
#425 = ADVANCED_BREP_SHAPE_REPRESENTATION('',(#439),#16938) ;
#426 = ADVANCED_BREP_SHAPE_REPRESENTATION('',(#440),#16939) ;
#427 = ADVANCED_BREP_SHAPE_REPRESENTATION('',(#441),#16940) ;
#428 = ADVANCED_BREP_SHAPE_REPRESENTATION('',(#442),#16941) ;
#429 = STYLED_ITEM('',(#17063),#436) ;
#430 = STYLED_ITEM('',(#17064),#437) ;
#431 = STYLED_ITEM('',(#17065),#438) ;
#432 = STYLED_ITEM('',(#17066),#439) ;
#433 = STYLED_ITEM('',(#17067),#440) ;
#434 = STYLED_ITEM('',(#17068),#441) ;
#435 = STYLED_ITEM('',(#17069),#442) ;
#436 = MANIFOLD_SOLID_BREP(
'Ball Spline Shaft No.16 x 120 Stepped D12 Tapped M8',#8178) ;
#437 = MANIFOLD_SOLID_BREP(
'Ball Spline Nut Outer Sleeve Round Flange BSLM16',#8179) ;
#438 = MANIFOLD_SOLID_BREP('Internal Ball Retainer Cage BSLM16',#8180) ;
#439 = MANIFOLD_SOLID_BREP('Precision Steel Ball D3.175 G10',#8181) ;
#440 = MANIFOLD_SOLID_BREP('ISO 4762 - M4 x 10 - 12.9',#8182) ;
#441 = MANIFOLD_SOLID_BREP('Wiper Rubber Seal BSLM16',#8183) ;
#442 = MANIFOLD_SOLID_BREP('DIN 472 - J24 x 1.2 Internal Retaining Ring',
#8184) ;
#443 = B_SPLINE_CURVE_WITH_KNOTS('',3,(#11023,#11024,#11025,#11026,#11027,
#11028),.UNSPECIFIED.,.F.,.F.,(4,2,4),(0.509460619201912,0.527252628402487,
0.551151897029291),.UNSPECIFIED.) ;
#444 = B_SPLINE_CURVE_WITH_KNOTS('',3,(#11032,#11033,#11034,#11035,#11036,
#11037,#11038),.UNSPECIFIED.,.F.,.F.,(4,3,4),(-0.0238992690166207,0.,0.0177920092005774),
 .UNSPECIFIED.) ;
#445 = B_SPLINE_CURVE_WITH_KNOTS('',3,(#11042,#11043,#11044,#11045,#11046,
#11047,#11048),.UNSPECIFIED.,.F.,.F.,(4,3,4),(-0.0177920090905049,0.,0.0238992686268042),
 .UNSPECIFIED.) ;
#446 = B_SPLINE_CURVE_WITH_KNOTS('',3,(#11052,#11053,#11054,#11055,#11056,
#11057),.UNSPECIFIED.,.F.,.F.,(4,2,4),(0.660208716959523,0.684107985586327,
0.701899994786901),.UNSPECIFIED.) ;
#447 = B_SPLINE_CURVE_WITH_KNOTS('',3,(#11062,#11063,#11064,#11065,#11066,
#11067),.UNSPECIFIED.,.F.,.F.,(4,2,4),(0.509460619201911,0.527252628402487,
0.55115189702929),.UNSPECIFIED.) ;
#448 = B_SPLINE_CURVE_WITH_KNOTS('',3,(#11071,#11072,#11073,#11074,#11075,
#11076,#11077),.UNSPECIFIED.,.F.,.F.,(4,3,4),(-0.0238992690166204,0.,0.0177920092005756),
 .UNSPECIFIED.) ;
#449 = B_SPLINE_CURVE_WITH_KNOTS('',3,(#11081,#11082,#11083,#11084,#11085,
#11086,#11087),.UNSPECIFIED.,.F.,.F.,(4,3,4),(-0.0177920090905051,0.,0.0238992686268041),
 .UNSPECIFIED.) ;
#450 = B_SPLINE_CURVE_WITH_KNOTS('',3,(#11091,#11092,#11093,#11094,#11095,
#11096),.UNSPECIFIED.,.F.,.F.,(4,2,4),(0.660208716959522,0.684107985586326,
0.701899994786901),.UNSPECIFIED.) ;
#451 = B_SPLINE_CURVE_WITH_KNOTS('',3,(#11101,#11102,#11103,#11104,#11105,
#11106,#11107),.UNSPECIFIED.,.F.,.F.,(4,3,4),(-0.0238992690166182,0.,0.0177920092005759),
 .UNSPECIFIED.) ;
#452 = B_SPLINE_CURVE_WITH_KNOTS('',3,(#11111,#11112,#11113,#11114,#11115,
#11116,#11117),.UNSPECIFIED.,.F.,.F.,(4,3,4),(-0.0177920090905041,0.,0.0238992686268048),
 .UNSPECIFIED.) ;
#453 = B_SPLINE_CURVE_WITH_KNOTS('',3,(#11121,#11122,#11123,#11124,#11125,
#11126),.UNSPECIFIED.,.F.,.F.,(4,2,4),(0.660208716959521,0.684107985586326,
0.701899994786899),.UNSPECIFIED.) ;
#454 = B_SPLINE_CURVE_WITH_KNOTS('',3,(#11130,#11131,#11132,#11133,#11134,
#11135),.UNSPECIFIED.,.F.,.F.,(4,2,4),(0.509460619201914,0.52725262840249,
0.551151897029293),.UNSPECIFIED.) ;
#455 = B_SPLINE_CURVE_WITH_KNOTS('',3,(#11140,#11141,#11142,#11143,#11144,
#11145,#11146),.UNSPECIFIED.,.F.,.F.,(4,3,4),(-0.0238992690166184,0.,0.0177920092005753),
 .UNSPECIFIED.) ;
#456 = B_SPLINE_CURVE_WITH_KNOTS('',3,(#11150,#11151,#11152,#11153,#11154,
#11155,#11156),.UNSPECIFIED.,.F.,.F.,(4,3,4),(-0.0177920090905042,0.,0.0238992686268048),
 .UNSPECIFIED.) ;
#457 = B_SPLINE_CURVE_WITH_KNOTS('',3,(#11160,#11161,#11162,#11163,#11164,
#11165),.UNSPECIFIED.,.F.,.F.,(4,2,4),(0.660208716959522,0.684107985586326,
0.7018999947869),.UNSPECIFIED.) ;
#458 = B_SPLINE_CURVE_WITH_KNOTS('',3,(#11169,#11170,#11171,#11172,#11173,
#11174),.UNSPECIFIED.,.F.,.F.,(4,2,4),(0.509460619201915,0.527252628402489,
0.551151897029294),.UNSPECIFIED.) ;
#459 = B_SPLINE_CURVE_WITH_KNOTS('',3,(#11232,#11233,#11234,#11235,#11236,
#11237,#11238,#11239,#11240,#11241),.UNSPECIFIED.,.F.,.F.,(4,3,3,4),(0.,
0.0150000164083537,0.0240853197637074,0.0337869872272911),.UNSPECIFIED.) ;
#460 = B_SPLINE_CURVE_WITH_KNOTS('',2,(#11245,#11246,#11247),
 .UNSPECIFIED.,.F.,.F.,(3,3),(0.,1.),.UNSPECIFIED.) ;
#461 = B_SPLINE_CURVE_WITH_KNOTS('',3,(#11256,#11257,#11258,#11259,#11260,
#11261,#11262,#11263,#11264,#11265),.UNSPECIFIED.,.F.,.F.,(4,3,3,4),(0.,
0.0173556832409861,0.0345243876037734,0.0405769411926334),.UNSPECIFIED.) ;
#462 = B_SPLINE_CURVE_WITH_KNOTS('',2,(#11267,#11268,#11269),
 .UNSPECIFIED.,.F.,.F.,(3,3),(0.,1.),.UNSPECIFIED.) ;
#463 = B_SPLINE_CURVE_WITH_KNOTS('',3,(#11278,#11279,#11280,#11281,#11282,
#11283,#11284,#11285,#11286,#11287),.UNSPECIFIED.,.F.,.F.,(4,3,3,4),(0.,
0.0206625445765638,0.029902214499977,0.0388796639931611),.UNSPECIFIED.) ;
#464 = B_SPLINE_CURVE_WITH_KNOTS('',2,(#11289,#11290,#11291),
 .UNSPECIFIED.,.F.,.F.,(3,3),(0.,1.),.UNSPECIFIED.) ;
#465 = B_SPLINE_CURVE_WITH_KNOTS('',3,(#11300,#11301,#11302,#11303,#11304,
#11305,#11306,#11307,#11308,#11309),.UNSPECIFIED.,.F.,.F.,(4,3,3,4),(0.,
0.0163020293322635,0.0252071380218071,0.0345773972689045),.UNSPECIFIED.) ;
#466 = B_SPLINE_CURVE_WITH_KNOTS('',2,(#11311,#11312,#11313),
 .UNSPECIFIED.,.F.,.F.,(3,3),(0.,1.),.UNSPECIFIED.) ;
#467 = B_SPLINE_CURVE_WITH_KNOTS('',3,(#11323,#11324,#11325,#11326,#11327,
#11328,#11329,#11330,#11331,#11332),.UNSPECIFIED.,.F.,.F.,(4,3,3,4),(0.,
0.0252144119583777,0.0382782631200122,0.0519544193610427),.UNSPECIFIED.) ;
#468 = B_SPLINE_CURVE_WITH_KNOTS('',2,(#11336,#11337,#11338),
 .UNSPECIFIED.,.F.,.F.,(3,3),(0.,1.),.UNSPECIFIED.) ;
#469 = B_SPLINE_CURVE_WITH_KNOTS('',3,(#11347,#11348,#11349,#11350,#11351,
#11352,#11353),.UNSPECIFIED.,.F.,.F.,(4,3,4),(0.,0.0265552382096679,0.0567118210565804),
 .UNSPECIFIED.) ;
#470 = B_SPLINE_CURVE_WITH_KNOTS('',2,(#11355,#11356,#11357),
 .UNSPECIFIED.,.F.,.F.,(3,3),(0.,1.),.UNSPECIFIED.) ;
#471 = B_SPLINE_CURVE_WITH_KNOTS('',3,(#11366,#11367,#11368,#11369,#11370,
#11371,#11372),.UNSPECIFIED.,.F.,.F.,(4,3,4),(0.,0.0202232312434472,0.0400735848175635),
 .UNSPECIFIED.) ;
#472 = B_SPLINE_CURVE_WITH_KNOTS('',2,(#11374,#11375,#11376),
 .UNSPECIFIED.,.F.,.F.,(3,3),(0.,1.),.UNSPECIFIED.) ;
#473 = B_SPLINE_CURVE_WITH_KNOTS('',3,(#11385,#11386,#11387,#11388,#11389,
#11390,#11391),.UNSPECIFIED.,.F.,.F.,(4,3,4),(0.,0.0190789474349663,0.0373947557586164),
 .UNSPECIFIED.) ;
#474 = B_SPLINE_CURVE_WITH_KNOTS('',2,(#11393,#11394,#11395),
 .UNSPECIFIED.,.F.,.F.,(3,3),(0.,1.),.UNSPECIFIED.) ;
#475 = B_SPLINE_CURVE_WITH_KNOTS('',3,(#11404,#11405,#11406,#11407,#11408,
#11409,#11410),.UNSPECIFIED.,.F.,.F.,(4,3,4),(0.,0.0182891079019429,0.0373295492055506),
 .UNSPECIFIED.) ;
#476 = B_SPLINE_CURVE_WITH_KNOTS('',2,(#11412,#11413,#11414),
 .UNSPECIFIED.,.F.,.F.,(3,3),(0.,1.),.UNSPECIFIED.) ;
#477 = B_SPLINE_CURVE_WITH_KNOTS('',3,(#11423,#11424,#11425,#11426,#11427,
#11428,#11429,#11430,#11431,#11432),.UNSPECIFIED.,.F.,.F.,(4,3,3,4),(0.,
0.0297542241681086,0.0460105236800287,0.0629020224502893),.UNSPECIFIED.) ;
#478 = B_SPLINE_CURVE_WITH_KNOTS('',2,(#11434,#11435,#11436),
 .UNSPECIFIED.,.F.,.F.,(3,3),(0.,1.),.UNSPECIFIED.) ;
#479 = B_SPLINE_CURVE_WITH_KNOTS('',3,(#11445,#11446,#11447,#11448,#11449,
#11450),.UNSPECIFIED.,.F.,.F.,(4,2,4),(0.,0.0242893868272739,0.0842237803126408),
 .UNSPECIFIED.) ;
#480 = B_SPLINE_CURVE_WITH_KNOTS('',2,(#11452,#11453,#11454),
 .UNSPECIFIED.,.F.,.F.,(3,3),(0.,1.),.UNSPECIFIED.) ;
#481 = B_SPLINE_CURVE_WITH_KNOTS('',3,(#11463,#11464,#11465,#11466,#11467,
#11468,#11469,#11470),.UNSPECIFIED.,.F.,.F.,(4,2,2,4),(0.,0.0544536973145401,
0.0767040245057299,0.0963873215037275),.UNSPECIFIED.) ;
#482 = B_SPLINE_CURVE_WITH_KNOTS('',2,(#11472,#11473,#11474),
 .UNSPECIFIED.,.F.,.F.,(3,3),(0.,1.),.UNSPECIFIED.) ;
#483 = B_SPLINE_CURVE_WITH_KNOTS('',3,(#11483,#11484,#11485,#11486,#11487,
#11488,#11489,#11490,#11491,#11492),.UNSPECIFIED.,.F.,.F.,(4,3,3,4),(0.,
0.0271232217099323,0.0446974737911228,0.0635054039669033),.UNSPECIFIED.) ;
#484 = B_SPLINE_CURVE_WITH_KNOTS('',2,(#11494,#11495,#11496),
 .UNSPECIFIED.,.F.,.F.,(3,3),(0.,1.),.UNSPECIFIED.) ;
#485 = B_SPLINE_CURVE_WITH_KNOTS('',3,(#11505,#11506,#11507,#11508,#11509,
#11510,#11511),.UNSPECIFIED.,.F.,.F.,(4,3,4),(0.,0.0175478594959351,0.0350949930523616),
 .UNSPECIFIED.) ;
#486 = B_SPLINE_CURVE_WITH_KNOTS('',2,(#11513,#11514,#11515),
 .UNSPECIFIED.,.F.,.F.,(3,3),(0.,1.),.UNSPECIFIED.) ;
#487 = B_SPLINE_CURVE_WITH_KNOTS('',3,(#11524,#11525,#11526,#11527,#11528,
#11529,#11530),.UNSPECIFIED.,.F.,.F.,(4,3,4),(0.,0.0121019216609115,0.0237901666703287),
 .UNSPECIFIED.) ;
#488 = B_SPLINE_CURVE_WITH_KNOTS('',2,(#11533,#11534,#11535),
 .UNSPECIFIED.,.F.,.F.,(3,3),(0.,1.),.UNSPECIFIED.) ;
#489 = B_SPLINE_CURVE_WITH_KNOTS('',3,(#11543,#11544,#11545,#11546,#11547,
#11548,#11549),.UNSPECIFIED.,.F.,.F.,(4,3,4),(0.,0.0133863918273521,0.0260692113791466),
 .UNSPECIFIED.) ;
#490 = B_SPLINE_CURVE_WITH_KNOTS('',2,(#11552,#11553,#11554),
 .UNSPECIFIED.,.F.,.F.,(3,3),(0.,1.),.UNSPECIFIED.) ;
#491 = B_SPLINE_CURVE_WITH_KNOTS('',3,(#11562,#11563,#11564,#11565,#11566,
#11567,#11568),.UNSPECIFIED.,.F.,.F.,(4,3,4),(0.,0.0138210255321488,0.0277017666505464),
 .UNSPECIFIED.) ;
#492 = B_SPLINE_CURVE_WITH_KNOTS('',2,(#11571,#11572,#11573),
 .UNSPECIFIED.,.F.,.F.,(3,3),(0.,1.),.UNSPECIFIED.) ;
#493 = B_SPLINE_CURVE_WITH_KNOTS('',3,(#11580,#11581,#11582,#11583,#11584,
#11585,#11586),.UNSPECIFIED.,.F.,.F.,(4,3,4),(0.,0.0173843205296013,0.0380243003929434),
 .UNSPECIFIED.) ;
#494 = B_SPLINE_CURVE_WITH_KNOTS('',2,(#11587,#11588,#11589),
 .UNSPECIFIED.,.F.,.F.,(3,3),(0.,1.),.UNSPECIFIED.) ;
#495 = B_SPLINE_CURVE_WITH_KNOTS('',3,(#11597,#11598,#11599,#11600,#11601,
#11602,#11603),.UNSPECIFIED.,.F.,.F.,(4,3,4),(0.,0.0240652575004504,0.0463449370279219),
 .UNSPECIFIED.) ;
#496 = B_SPLINE_CURVE_WITH_KNOTS('',2,(#11605,#11606,#11607),
 .UNSPECIFIED.,.F.,.F.,(3,3),(0.,1.),.UNSPECIFIED.) ;
#497 = B_SPLINE_CURVE_WITH_KNOTS('',3,(#11616,#11617,#11618,#11619,#11620,
#11621,#11622),.UNSPECIFIED.,.F.,.F.,(4,3,4),(0.,0.0155188224962534,0.0308533680520038),
 .UNSPECIFIED.) ;
#498 = B_SPLINE_CURVE_WITH_KNOTS('',2,(#11625,#11626,#11627),
 .UNSPECIFIED.,.F.,.F.,(3,3),(0.,1.),.UNSPECIFIED.) ;
#499 = B_SPLINE_CURVE_WITH_KNOTS('',3,(#11635,#11636,#11637,#11638,#11639,
#11640,#11641),.UNSPECIFIED.,.F.,.F.,(4,3,4),(0.,0.0169672680417701,0.0330071131092539),
 .UNSPECIFIED.) ;
#500 = B_SPLINE_CURVE_WITH_KNOTS('',2,(#11644,#11645,#11646),
 .UNSPECIFIED.,.F.,.F.,(3,3),(0.,1.),.UNSPECIFIED.) ;
#501 = B_SPLINE_CURVE_WITH_KNOTS('',3,(#11654,#11655,#11656,#11657,#11658,
#11659,#11660,#11661,#11662,#11663,#11664,#11665,#11666),.UNSPECIFIED.,
 .F.,.F.,(4,3,3,3,4),(0.,0.011770749270626,0.0219604401624206,0.0415400615610363,
0.0508377264422704),.UNSPECIFIED.) ;
#502 = B_SPLINE_CURVE_WITH_KNOTS('',2,(#11669,#11670,#11671),
 .UNSPECIFIED.,.F.,.F.,(3,3),(0.,1.),.UNSPECIFIED.) ;
#503 = B_SPLINE_CURVE_WITH_KNOTS('',3,(#11679,#11680,#11681,#11682,#11683,
#11684,#11685),.UNSPECIFIED.,.F.,.F.,(4,3,4),(0.,0.0163246527969622,0.0343462180387076),
 .UNSPECIFIED.) ;
#504 = B_SPLINE_CURVE_WITH_KNOTS('',2,(#11688,#11689,#11690),
 .UNSPECIFIED.,.F.,.F.,(3,3),(0.,1.),.UNSPECIFIED.) ;
#505 = B_SPLINE_CURVE_WITH_KNOTS('',3,(#11698,#11699,#11700,#11701,#11702,
#11703,#11704),.UNSPECIFIED.,.F.,.F.,(4,3,4),(0.,0.0123718787780963,0.0243811015603076),
 .UNSPECIFIED.) ;
#506 = B_SPLINE_CURVE_WITH_KNOTS('',2,(#11707,#11708,#11709),
 .UNSPECIFIED.,.F.,.F.,(3,3),(0.,1.),.UNSPECIFIED.) ;
#507 = B_SPLINE_CURVE_WITH_KNOTS('',3,(#11717,#11718,#11719,#11720,#11721,
#11722,#11723,#11724,#11725,#11726),.UNSPECIFIED.,.F.,.F.,(4,3,3,4),(0.,
0.0148349366343986,0.0224838356253581,0.0304748092482181),.UNSPECIFIED.) ;
#508 = B_SPLINE_CURVE_WITH_KNOTS('',2,(#11729,#11730,#11731),
 .UNSPECIFIED.,.F.,.F.,(3,3),(0.,1.),.UNSPECIFIED.) ;
#509 = B_SPLINE_CURVE_WITH_KNOTS('',3,(#11739,#11740,#11741,#11742,#11743,
#11744,#11745,#11746,#11747,#11748,#11749,#11750,#11751),.UNSPECIFIED.,
 .F.,.F.,(4,3,3,3,4),(0.,0.0130698557907629,0.0141731149392098,0.0234680574806899,
0.0251327017063842),.UNSPECIFIED.) ;
#510 = B_SPLINE_CURVE_WITH_KNOTS('',2,(#11754,#11755,#11756),
 .UNSPECIFIED.,.F.,.F.,(3,3),(0.,1.),.UNSPECIFIED.) ;
#511 = B_SPLINE_CURVE_WITH_KNOTS('',3,(#11769,#11770,#11771,#11772,#11773,
#11774,#11775),.UNSPECIFIED.,.F.,.F.,(4,3,4),(0.,0.0222485092698476,0.0462903807438163),
 .UNSPECIFIED.) ;
#512 = B_SPLINE_CURVE_WITH_KNOTS('',2,(#11776,#11777,#11778),
 .UNSPECIFIED.,.F.,.F.,(3,3),(0.,1.),.UNSPECIFIED.) ;
#513 = B_SPLINE_CURVE_WITH_KNOTS('',3,(#11788,#11789,#11790,#11791,#11792,
#11793,#11794),.UNSPECIFIED.,.F.,.F.,(4,3,4),(0.,0.0169828382589056,0.0314916243151362),
 .UNSPECIFIED.) ;
#514 = B_SPLINE_CURVE_WITH_KNOTS('',2,(#11798,#11799,#11800),
 .UNSPECIFIED.,.F.,.F.,(3,3),(0.,1.),.UNSPECIFIED.) ;
#515 = B_SPLINE_CURVE_WITH_KNOTS('',3,(#11815,#11816,#11817,#11818,#11819,
#11820,#11821),.UNSPECIFIED.,.F.,.F.,(4,3,4),(0.,0.024316559375796,0.0475130234788273),
 .UNSPECIFIED.) ;
#516 = B_SPLINE_CURVE_WITH_KNOTS('',2,(#11823,#11824,#11825),
 .UNSPECIFIED.,.F.,.F.,(3,3),(0.,1.),.UNSPECIFIED.) ;
#517 = B_SPLINE_CURVE_WITH_KNOTS('',3,(#11834,#11835,#11836,#11837,#11838,
#11839,#11840),.UNSPECIFIED.,.F.,.F.,(4,3,4),(0.,0.0206525582993816,0.0379545073521461),
 .UNSPECIFIED.) ;
#518 = B_SPLINE_CURVE_WITH_KNOTS('',2,(#11842,#11843,#11844),
 .UNSPECIFIED.,.F.,.F.,(3,3),(0.,1.),.UNSPECIFIED.) ;
#519 = B_SPLINE_CURVE_WITH_KNOTS('',3,(#11859,#11860,#11861,#11862,#11863,
#11864,#11865),.UNSPECIFIED.,.F.,.F.,(4,3,4),(0.,0.014536996568322,0.0315221142844197),
 .UNSPECIFIED.) ;
#520 = B_SPLINE_CURVE_WITH_KNOTS('',2,(#11868,#11869,#11870),
 .UNSPECIFIED.,.F.,.F.,(3,3),(0.,1.),.UNSPECIFIED.) ;
#521 = B_SPLINE_CURVE_WITH_KNOTS('',3,(#11905,#11906,#11907,#11908,#11909,
#11910,#11911,#11912,#11913,#11914,#11915,#11916,#11917,#11918,#11919,#11920,
#11921,#11922,#11923,#11924,#11925,#11926,#11927,#11928,#11929),
 .UNSPECIFIED.,.F.,.F.,(4,3,3,3,3,3,3,3,4),(0.,0.00569194123592617,0.0112324310971198,
0.0165429389179945,0.0201111003725969,0.0242173233513949,0.0282108821611355,
0.0320493450397511,0.0344815069837439),.UNSPECIFIED.) ;
#522 = B_SPLINE_CURVE_WITH_KNOTS('',3,(#11931,#11932,#11933,#11934,#11935,
#11936,#11937,#11938,#11939,#11940,#11941,#11942,#11943,#11944,#11945,#11946,
#11947,#11948,#11949,#11950,#11951,#11952,#11953,#11954,#11955),
 .UNSPECIFIED.,.F.,.F.,(4,3,3,3,3,3,3,3,4),(0.,0.00418301047252267,0.00846262474705522,
0.0129021161814928,0.0149322544938229,0.0205445093223957,0.0263037117443392,
0.0322933826159474,0.0355643359068167),.UNSPECIFIED.) ;
#523 = B_SPLINE_CURVE_WITH_KNOTS('',3,(#11973,#11974,#11975,#11976,#11977,
#11978,#11979),.UNSPECIFIED.,.F.,.F.,(4,3,4),(0.,0.0212364832794801,0.0419899948755705),
 .UNSPECIFIED.) ;
#524 = B_SPLINE_CURVE_WITH_KNOTS('',3,(#11981,#11982,#11983,#11984,#11985,
#11986,#11987),.UNSPECIFIED.,.F.,.F.,(4,3,4),(0.,0.0207952315113147,0.0421638470613952),
 .UNSPECIFIED.) ;
#525 = B_SPLINE_CURVE_WITH_KNOTS('',3,(#11991,#11992,#11993,#11994,#11995,
#11996,#11997),.UNSPECIFIED.,.F.,.F.,(4,3,4),(0.,0.0153442120866379,0.0288161992642492),
 .UNSPECIFIED.) ;
#526 = B_SPLINE_CURVE_WITH_KNOTS('',3,(#11999,#12000,#12001,#12002,#12003,
#12004,#12005),.UNSPECIFIED.,.F.,.F.,(4,3,4),(0.,0.0133416659410013,0.0284117643200023),
 .UNSPECIFIED.) ;
#527 = B_SPLINE_CURVE_WITH_KNOTS('',3,(#12007,#12008,#12009,#12010,#12011,
#12012,#12013),.UNSPECIFIED.,.F.,.F.,(4,3,4),(0.,0.0167683780422157,0.034705436927841),
 .UNSPECIFIED.) ;
#528 = B_SPLINE_CURVE_WITH_KNOTS('',3,(#12015,#12016,#12017,#12018,#12019,
#12020,#12021),.UNSPECIFIED.,.F.,.F.,(4,3,4),(0.,0.0157245600444115,0.0299896116808996),
 .UNSPECIFIED.) ;
#529 = B_SPLINE_CURVE_WITH_KNOTS('',3,(#12023,#12024,#12025,#12026,#12027,
#12028,#12029),.UNSPECIFIED.,.F.,.F.,(4,3,4),(0.,0.0125773378818699,0.0237065110114582),
 .UNSPECIFIED.) ;
#530 = B_SPLINE_CURVE_WITH_KNOTS('',3,(#12031,#12032,#12033,#12034,#12035,
#12036,#12037),.UNSPECIFIED.,.F.,.F.,(4,3,4),(0.,0.0102693084451865,0.0203354088326608),
 .UNSPECIFIED.) ;
#531 = B_SPLINE_CURVE_WITH_KNOTS('',3,(#12039,#12040,#12041,#12042,#12043,
#12044,#12045),.UNSPECIFIED.,.F.,.F.,(4,3,4),(0.,0.00992200971474841,0.0195786738962378),
 .UNSPECIFIED.) ;
#532 = B_SPLINE_CURVE_WITH_KNOTS('',3,(#12047,#12048,#12049,#12050,#12051,
#12052,#12053,#12054,#12055,#12056),.UNSPECIFIED.,.F.,.F.,(4,3,3,4),(0.,
0.0106013294774732,0.0222845622588424,0.023809317348732),.UNSPECIFIED.) ;
#533 = B_SPLINE_CURVE_WITH_KNOTS('',3,(#12058,#12059,#12060,#12061,#12062,
#12063,#12064,#12065,#12066,#12067,#12068,#12069,#12070,#12071,#12072,#12073,
#12074,#12075,#12076),.UNSPECIFIED.,.F.,.F.,(4,3,3,3,3,3,4),(0.,0.00590422965020825,
0.00941919373558824,0.0118084593004165,0.0183919439982395,0.0279075522839463,
0.0311693981304476),.UNSPECIFIED.) ;
#534 = B_SPLINE_CURVE_WITH_KNOTS('',3,(#12078,#12079,#12080,#12081,#12082,
#12083,#12084,#12085,#12086,#12087,#12088,#12089,#12090),.UNSPECIFIED.,
 .F.,.F.,(4,3,3,3,4),(0.,0.0150109515841417,0.0257666496332491,0.0333691467947793,
0.0442792551451376),.UNSPECIFIED.) ;
#535 = B_SPLINE_CURVE_WITH_KNOTS('',3,(#12092,#12093,#12094,#12095,#12096,
#12097,#12098),.UNSPECIFIED.,.F.,.F.,(4,3,4),(0.,0.016591534262115,0.0315880473127885),
 .UNSPECIFIED.) ;
#536 = B_SPLINE_CURVE_WITH_KNOTS('',3,(#12100,#12101,#12102,#12103,#12104,
#12105,#12106),.UNSPECIFIED.,.F.,.F.,(4,3,4),(0.,0.0143488858698759,0.0290305106878466),
 .UNSPECIFIED.) ;
#537 = B_SPLINE_CURVE_WITH_KNOTS('',3,(#12108,#12109,#12110,#12111,#12112,
#12113,#12114),.UNSPECIFIED.,.F.,.F.,(4,3,4),(0.,0.0164683028045611,0.0332538948383704),
 .UNSPECIFIED.) ;
#538 = B_SPLINE_CURVE_WITH_KNOTS('',3,(#12116,#12117,#12118,#12119,#12120,
#12121,#12122),.UNSPECIFIED.,.F.,.F.,(4,3,4),(0.,0.017474633999681,0.0360764640896449),
 .UNSPECIFIED.) ;
#539 = B_SPLINE_CURVE_WITH_KNOTS('',3,(#12124,#12125,#12126,#12127,#12128,
#12129,#12130),.UNSPECIFIED.,.F.,.F.,(4,3,4),(0.,0.0200770342233018,0.0414114209213859),
 .UNSPECIFIED.) ;
#540 = B_SPLINE_CURVE_WITH_KNOTS('',3,(#12132,#12133,#12134,#12135,#12136,
#12137,#12138),.UNSPECIFIED.,.F.,.F.,(4,3,4),(0.,0.0231080610840433,0.0441729224541179),
 .UNSPECIFIED.) ;
#541 = B_SPLINE_CURVE_WITH_KNOTS('',3,(#12140,#12141,#12142,#12143,#12144,
#12145,#12146),.UNSPECIFIED.,.F.,.F.,(4,3,4),(0.,0.0193208384469699,0.037730112389279),
 .UNSPECIFIED.) ;
#542 = B_SPLINE_CURVE_WITH_KNOTS('',3,(#12148,#12149,#12150,#12151,#12152,
#12153,#12154),.UNSPECIFIED.,.F.,.F.,(4,3,4),(0.,0.0182396170597861,0.0370031988263464),
 .UNSPECIFIED.) ;
#543 = B_SPLINE_CURVE_WITH_KNOTS('',3,(#12158,#12159,#12160,#12161,#12162,
#12163,#12164,#12165,#12166,#12167),.UNSPECIFIED.,.F.,.F.,(4,3,3,4),(0.,
0.0190427568358624,0.0276047621343949,0.0359942554921667),.UNSPECIFIED.) ;
#544 = B_SPLINE_CURVE_WITH_KNOTS('',3,(#12169,#12170,#12171,#12172,#12173,
#12174,#12175,#12176,#12177,#12178),.UNSPECIFIED.,.F.,.F.,(4,3,3,4),(0.,
0.0145175548511501,0.0262513287029716,0.0402671823708522),.UNSPECIFIED.) ;
#545 = B_SPLINE_CURVE_WITH_KNOTS('',3,(#12180,#12181,#12182,#12183,#12184,
#12185,#12186,#12187,#12188,#12189,#12190,#12191,#12192),.UNSPECIFIED.,
 .F.,.F.,(4,3,3,3,4),(0.,0.0151398944763002,0.0225141408320645,0.031716815308806,
0.0398561587170203),.UNSPECIFIED.) ;
#546 = B_SPLINE_CURVE_WITH_KNOTS('',3,(#12194,#12195,#12196,#12197,#12198,
#12199,#12200,#12201,#12202,#12203),.UNSPECIFIED.,.F.,.F.,(4,3,3,4),(0.,
0.0134998512216097,0.0203874514613731,0.0273913827533458),.UNSPECIFIED.) ;
#547 = B_SPLINE_CURVE_WITH_KNOTS('',3,(#12205,#12206,#12207,#12208,#12209,
#12210,#12211,#12212,#12213,#12214),.UNSPECIFIED.,.F.,.F.,(4,3,3,4),(0.,
0.0107582822420351,0.016345486370408,0.0221382733736323),.UNSPECIFIED.) ;
#548 = B_SPLINE_CURVE_WITH_KNOTS('',3,(#12216,#12217,#12218,#12219,#12220,
#12221,#12222,#12223,#12224,#12225,#12226,#12227,#12228,#12229,#12230,#12231),
 .UNSPECIFIED.,.F.,.F.,(4,3,3,3,3,4),(0.,0.00420466729910508,0.00633552272142135,
0.0165957853018843,0.0257546857993008,0.031100367807991),.UNSPECIFIED.) ;
#549 = B_SPLINE_CURVE_WITH_KNOTS('',3,(#12233,#12234,#12235,#12236,#12237,
#12238,#12239,#12240,#12241,#12242,#12243,#12244,#12245,#12246,#12247,#12248,
#12249,#12250,#12251),.UNSPECIFIED.,.F.,.F.,(4,3,3,3,3,3,4),(0.,0.0140462067224565,
0.0254132340708786,0.0295355002228338,0.0368102718442848,0.0465126418826644,
0.0498614406746093),.UNSPECIFIED.) ;
#550 = B_SPLINE_CURVE_WITH_KNOTS('',3,(#12253,#12254,#12255,#12256,#12257,
#12258,#12259),.UNSPECIFIED.,.F.,.F.,(4,3,4),(0.,0.0194616671587977,0.0366325539762354),
 .UNSPECIFIED.) ;
#551 = B_SPLINE_CURVE_WITH_KNOTS('',3,(#12261,#12262,#12263,#12264,#12265,
#12266,#12267),.UNSPECIFIED.,.F.,.F.,(4,3,4),(0.,0.0163404825673663,0.0333147063175432),
 .UNSPECIFIED.) ;
#552 = B_SPLINE_CURVE_WITH_KNOTS('',3,(#12269,#12270,#12271,#12272,#12273,
#12274,#12275),.UNSPECIFIED.,.F.,.F.,(4,3,4),(0.,0.0174292102142414,0.0353223313086727),
 .UNSPECIFIED.) ;
#553 = B_SPLINE_CURVE_WITH_KNOTS('',3,(#12277,#12278,#12279,#12280,#12281,
#12282,#12283),.UNSPECIFIED.,.F.,.F.,(4,3,4),(0.,0.0186689879508952,0.03840958766807),
 .UNSPECIFIED.) ;
#554 = B_SPLINE_CURVE_WITH_KNOTS('',3,(#12285,#12286,#12287,#12288,#12289,
#12290,#12291),.UNSPECIFIED.,.F.,.F.,(4,3,4),(0.,0.0211615752193719,0.0437139193650708),
 .UNSPECIFIED.) ;
#555 = B_SPLINE_CURVE_WITH_KNOTS('',3,(#12292,#12293,#12294,#12295,#12296,
#12297,#12298),.UNSPECIFIED.,.F.,.F.,(4,3,4),(0.,0.0274003599038337,0.0509298041237331),
 .UNSPECIFIED.) ;
#556 = B_SPLINE_CURVE_WITH_KNOTS('',3,(#12301,#12302,#12303,#12304,#12305,
#12306,#12307,#12308,#12309,#12310,#12311,#12312,#12313,#12314,#12315,#12316),
 .UNSPECIFIED.,.F.,.F.,(4,3,3,3,3,4),(0.,0.0119556380038084,0.0224119134293328,
0.0318321821221747,0.0533934645702515,0.0580324870841514),.UNSPECIFIED.) ;
#557 = B_SPLINE_CURVE_WITH_KNOTS('',3,(#12324,#12325,#12326,#12327,#12328,
#12329,#12330,#12331,#12332,#12333,#12334,#12335,#12336),.UNSPECIFIED.,
 .F.,.F.,(4,3,3,3,4),(0.,0.0189611702963205,0.0294450271990619,0.0495973866637977,
0.0527785820105709),.UNSPECIFIED.) ;
#558 = B_SPLINE_CURVE_WITH_KNOTS('',3,(#12338,#12339,#12340,#12341,#12342,
#12343,#12344),.UNSPECIFIED.,.F.,.F.,(4,3,4),(0.,0.0208854143008092,0.0428246780067487),
 .UNSPECIFIED.) ;
#559 = B_SPLINE_CURVE_WITH_KNOTS('',3,(#12346,#12347,#12348,#12349,#12350,
#12351,#12352,#12353,#12354,#12355),.UNSPECIFIED.,.F.,.F.,(4,3,3,4),(0.,
0.0246117446194239,0.0505233392813415,0.0534405730663183),.UNSPECIFIED.) ;
#560 = B_SPLINE_CURVE_WITH_KNOTS('',3,(#12357,#12358,#12359,#12360,#12361,
#12362,#12363),.UNSPECIFIED.,.F.,.F.,(4,3,4),(0.,0.0280864188477132,0.0520232165124005),
 .UNSPECIFIED.) ;
#561 = B_SPLINE_CURVE_WITH_KNOTS('',3,(#12365,#12366,#12367,#12368,#12369,
#12370,#12371),.UNSPECIFIED.,.F.,.F.,(4,3,4),(0.,0.0215752408071767,0.0429475903985937),
 .UNSPECIFIED.) ;
#562 = B_SPLINE_CURVE_WITH_KNOTS('',3,(#12373,#12374,#12375,#12376,#12377,
#12378,#12379,#12380,#12381,#12382,#12383,#12384,#12385),.UNSPECIFIED.,
 .F.,.F.,(4,3,3,3,4),(0.,0.0161321376565823,0.0244265641217521,0.0465899314620809,
0.055430671682033),.UNSPECIFIED.) ;
#563 = B_SPLINE_CURVE_WITH_KNOTS('',3,(#12393,#12394,#12395,#12396,#12397,
#12398,#12399,#12400,#12401,#12402,#12403,#12404,#12405,#12406,#12407,#12408),
 .UNSPECIFIED.,.F.,.F.,(4,3,3,3,3,4),(0.,0.0114819968961422,0.0243079810619617,
0.0325847915710728,0.0396674571422663,0.0414198473083807),.UNSPECIFIED.) ;
#564 = B_SPLINE_CURVE_WITH_KNOTS('',3,(#12410,#12411,#12412,#12413,#12414,
#12415,#12416),.UNSPECIFIED.,.F.,.F.,(4,3,4),(0.,0.0142419556450609,0.0286422433204278),
 .UNSPECIFIED.) ;
#565 = B_SPLINE_CURVE_WITH_KNOTS('',3,(#12418,#12419,#12420,#12421,#12422,
#12423,#12424),.UNSPECIFIED.,.F.,.F.,(4,3,4),(0.,0.0155686949793599,0.0329892430022521),
 .UNSPECIFIED.) ;
#566 = B_SPLINE_CURVE_WITH_KNOTS('',3,(#12425,#12426,#12427,#12428,#12429,
#12430,#12431,#12432,#12433,#12434,#12435,#12436,#12437),.UNSPECIFIED.,
 .F.,.F.,(4,3,3,3,4),(0.,0.0168788660747152,0.0272942730411942,0.0385456173339853,
0.0488240973210902),.UNSPECIFIED.) ;
#567 = B_SPLINE_CURVE_WITH_KNOTS('',3,(#12450,#12451,#12452,#12453,#12454,
#12455,#12456,#12457,#12458,#12459,#12460,#12461,#12462,#12463,#12464,#12465,
#12466,#12467,#12468,#12469,#12470,#12471,#12472,#12473,#12474),
 .UNSPECIFIED.,.F.,.F.,(4,3,3,3,3,3,3,3,4),(0.,0.00569194898760575,0.01123244639831,
0.016542961918724,0.0201111017205057,0.0242173359611551,0.0282109067622345,
0.0320493831348753,0.0344815023961872),.UNSPECIFIED.) ;
#568 = B_SPLINE_CURVE_WITH_KNOTS('',3,(#12476,#12477,#12478,#12479,#12480,
#12481,#12482,#12483,#12484,#12485,#12486,#12487,#12488,#12489,#12490,#12491,
#12492,#12493,#12494,#12495,#12496,#12497,#12498,#12499,#12500),
 .UNSPECIFIED.,.F.,.F.,(4,3,3,3,3,3,3,3,4),(0.,0.0041831224210667,0.00846284315641277,
0.0129024287836777,0.0149322446600846,0.0205445691292746,0.026303841906127,
0.0322935838006437,0.0355643694351932),.UNSPECIFIED.) ;
#569 = B_SPLINE_CURVE_WITH_KNOTS('',2,(#12612,#12613,#12614),
 .UNSPECIFIED.,.F.,.F.,(3,3),(0.,1.),.UNSPECIFIED.) ;
#570 = B_SPLINE_CURVE_WITH_KNOTS('',2,(#12623,#12624,#12625),
 .UNSPECIFIED.,.F.,.F.,(3,3),(0.,1.),.UNSPECIFIED.) ;
#571 = B_SPLINE_CURVE_WITH_KNOTS('',2,(#12650,#12651,#12652),
 .UNSPECIFIED.,.F.,.F.,(3,3),(0.,1.),.UNSPECIFIED.) ;
#572 = B_SPLINE_CURVE_WITH_KNOTS('',2,(#12673,#12674,#12675),
 .UNSPECIFIED.,.F.,.F.,(3,3),(0.,1.),.UNSPECIFIED.) ;
#573 = B_SPLINE_CURVE_WITH_KNOTS('',2,(#12684,#12685,#12686),
 .UNSPECIFIED.,.F.,.F.,(3,3),(0.,1.),.UNSPECIFIED.) ;
#574 = B_SPLINE_CURVE_WITH_KNOTS('',2,(#12695,#12696,#12697),
 .UNSPECIFIED.,.F.,.F.,(3,3),(0.,1.),.UNSPECIFIED.) ;
#575 = B_SPLINE_CURVE_WITH_KNOTS('',2,(#12706,#12707,#12708),
 .UNSPECIFIED.,.F.,.F.,(3,3),(0.,1.),.UNSPECIFIED.) ;
#576 = B_SPLINE_CURVE_WITH_KNOTS('',2,(#12717,#12718,#12719),
 .UNSPECIFIED.,.F.,.F.,(3,3),(0.,1.),.UNSPECIFIED.) ;
#577 = B_SPLINE_CURVE_WITH_KNOTS('',2,(#12729,#12730,#12731),
 .UNSPECIFIED.,.F.,.F.,(3,3),(0.,1.),.UNSPECIFIED.) ;
#578 = B_SPLINE_CURVE_WITH_KNOTS('',2,(#12740,#12741,#12742),
 .UNSPECIFIED.,.F.,.F.,(3,3),(0.,1.),.UNSPECIFIED.) ;
#579 = B_SPLINE_CURVE_WITH_KNOTS('',2,(#12751,#12752,#12753),
 .UNSPECIFIED.,.F.,.F.,(3,3),(0.,1.),.UNSPECIFIED.) ;
#580 = B_SPLINE_CURVE_WITH_KNOTS('',2,(#12762,#12763,#12764),
 .UNSPECIFIED.,.F.,.F.,(3,3),(0.,1.),.UNSPECIFIED.) ;
#581 = B_SPLINE_CURVE_WITH_KNOTS('',2,(#12773,#12774,#12775),
 .UNSPECIFIED.,.F.,.F.,(3,3),(0.,1.),.UNSPECIFIED.) ;
#582 = B_SPLINE_CURVE_WITH_KNOTS('',2,(#12796,#12797,#12798),
 .UNSPECIFIED.,.F.,.F.,(3,3),(0.,1.),.UNSPECIFIED.) ;
#583 = B_SPLINE_CURVE_WITH_KNOTS('',2,(#12807,#12808,#12809),
 .UNSPECIFIED.,.F.,.F.,(3,3),(0.,1.),.UNSPECIFIED.) ;
#584 = B_SPLINE_CURVE_WITH_KNOTS('',2,(#12818,#12819,#12820),
 .UNSPECIFIED.,.F.,.F.,(3,3),(0.,1.),.UNSPECIFIED.) ;
#585 = B_SPLINE_CURVE_WITH_KNOTS('',2,(#12833,#12834,#12835),
 .UNSPECIFIED.,.F.,.F.,(3,3),(0.,1.),.UNSPECIFIED.) ;
#586 = B_SPLINE_CURVE_WITH_KNOTS('',2,(#12844,#12845,#12846),
 .UNSPECIFIED.,.F.,.F.,(3,3),(0.,1.),.UNSPECIFIED.) ;
#587 = B_SPLINE_CURVE_WITH_KNOTS('',2,(#12855,#12856,#12857),
 .UNSPECIFIED.,.F.,.F.,(3,3),(0.,1.),.UNSPECIFIED.) ;
#588 = B_SPLINE_CURVE_WITH_KNOTS('',2,(#12866,#12867,#12868),
 .UNSPECIFIED.,.F.,.F.,(3,3),(0.,1.),.UNSPECIFIED.) ;
#589 = B_SPLINE_CURVE_WITH_KNOTS('',2,(#12877,#12878,#12879),
 .UNSPECIFIED.,.F.,.F.,(3,3),(0.,1.),.UNSPECIFIED.) ;
#590 = B_SPLINE_CURVE_WITH_KNOTS('',2,(#12888,#12889,#12890),
 .UNSPECIFIED.,.F.,.F.,(3,3),(0.,1.),.UNSPECIFIED.) ;
#591 = B_SPLINE_CURVE_WITH_KNOTS('',2,(#12899,#12900,#12901),
 .UNSPECIFIED.,.F.,.F.,(3,3),(0.,1.),.UNSPECIFIED.) ;
#592 = B_SPLINE_CURVE_WITH_KNOTS('',2,(#12910,#12911,#12912),
 .UNSPECIFIED.,.F.,.F.,(3,3),(0.,1.),.UNSPECIFIED.) ;
#593 = B_SPLINE_CURVE_WITH_KNOTS('',2,(#12921,#12922,#12923),
 .UNSPECIFIED.,.F.,.F.,(3,3),(0.,1.),.UNSPECIFIED.) ;
#594 = B_SPLINE_CURVE_WITH_KNOTS('',2,(#12932,#12933,#12934),
 .UNSPECIFIED.,.F.,.F.,(3,3),(0.,1.),.UNSPECIFIED.) ;
#595 = B_SPLINE_CURVE_WITH_KNOTS('',2,(#12943,#12944,#12945),
 .UNSPECIFIED.,.F.,.F.,(3,3),(0.,1.),.UNSPECIFIED.) ;
#596 = B_SPLINE_CURVE_WITH_KNOTS('',2,(#12954,#12955,#12956),
 .UNSPECIFIED.,.F.,.F.,(3,3),(0.,1.),.UNSPECIFIED.) ;
#597 = B_SPLINE_CURVE_WITH_KNOTS('',2,(#12965,#12966,#12967),
 .UNSPECIFIED.,.F.,.F.,(3,3),(0.,1.),.UNSPECIFIED.) ;
#598 = B_SPLINE_CURVE_WITH_KNOTS('',2,(#12976,#12977,#12978),
 .UNSPECIFIED.,.F.,.F.,(3,3),(0.,1.),.UNSPECIFIED.) ;
#599 = B_SPLINE_CURVE_WITH_KNOTS('',2,(#12988,#12989,#12990),
 .UNSPECIFIED.,.F.,.F.,(3,3),(0.,1.),.UNSPECIFIED.) ;
#600 = B_SPLINE_CURVE_WITH_KNOTS('',2,(#12999,#13000,#13001),
 .UNSPECIFIED.,.F.,.F.,(3,3),(0.,1.),.UNSPECIFIED.) ;
#601 = B_SPLINE_CURVE_WITH_KNOTS('',2,(#13010,#13011,#13012),
 .UNSPECIFIED.,.F.,.F.,(3,3),(0.,1.),.UNSPECIFIED.) ;
#602 = B_SPLINE_CURVE_WITH_KNOTS('',2,(#13021,#13022,#13023),
 .UNSPECIFIED.,.F.,.F.,(3,3),(0.,1.),.UNSPECIFIED.) ;
#603 = B_SPLINE_CURVE_WITH_KNOTS('',2,(#13032,#13033,#13034),
 .UNSPECIFIED.,.F.,.F.,(3,3),(0.,1.),.UNSPECIFIED.) ;
#604 = B_SPLINE_CURVE_WITH_KNOTS('',2,(#13043,#13044,#13045),
 .UNSPECIFIED.,.F.,.F.,(3,3),(0.,1.),.UNSPECIFIED.) ;
#605 = B_SPLINE_CURVE_WITH_KNOTS('',2,(#13054,#13055,#13056),
 .UNSPECIFIED.,.F.,.F.,(3,3),(0.,1.),.UNSPECIFIED.) ;
#606 = B_SPLINE_CURVE_WITH_KNOTS('',2,(#13065,#13066,#13067),
 .UNSPECIFIED.,.F.,.F.,(3,3),(0.,1.),.UNSPECIFIED.) ;
#607 = B_SPLINE_CURVE_WITH_KNOTS('',2,(#13076,#13077,#13078),
 .UNSPECIFIED.,.F.,.F.,(3,3),(0.,1.),.UNSPECIFIED.) ;
#608 = B_SPLINE_CURVE_WITH_KNOTS('',2,(#13087,#13088,#13089),
 .UNSPECIFIED.,.F.,.F.,(3,3),(0.,1.),.UNSPECIFIED.) ;
#609 = B_SPLINE_CURVE_WITH_KNOTS('',2,(#13098,#13099,#13100),
 .UNSPECIFIED.,.F.,.F.,(3,3),(0.,1.),.UNSPECIFIED.) ;
#610 = B_SPLINE_CURVE_WITH_KNOTS('',2,(#13109,#13110,#13111),
 .UNSPECIFIED.,.F.,.F.,(3,3),(0.,1.),.UNSPECIFIED.) ;
#611 = B_SPLINE_CURVE_WITH_KNOTS('',2,(#13120,#13121,#13122),
 .UNSPECIFIED.,.F.,.F.,(3,3),(0.,1.),.UNSPECIFIED.) ;
#612 = B_SPLINE_CURVE_WITH_KNOTS('',2,(#13131,#13132,#13133),
 .UNSPECIFIED.,.F.,.F.,(3,3),(0.,1.),.UNSPECIFIED.) ;
#613 = B_SPLINE_CURVE_WITH_KNOTS('',2,(#13142,#13143,#13144),
 .UNSPECIFIED.,.F.,.F.,(3,3),(0.,1.),.UNSPECIFIED.) ;
#614 = B_SPLINE_CURVE_WITH_KNOTS('',2,(#13155,#13156,#13157),
 .UNSPECIFIED.,.F.,.F.,(3,3),(0.,1.),.UNSPECIFIED.) ;
#615 = B_SPLINE_CURVE_WITH_KNOTS('',2,(#13205,#13206,#13207),
 .UNSPECIFIED.,.F.,.F.,(3,3),(0.,1.),.UNSPECIFIED.) ;
#616 = B_SPLINE_CURVE_WITH_KNOTS('',2,(#13216,#13217,#13218),
 .UNSPECIFIED.,.F.,.F.,(3,3),(0.,1.),.UNSPECIFIED.) ;
#617 = B_SPLINE_CURVE_WITH_KNOTS('',3,(#13280,#13281,#13282,#13283,#13284,
#13285),.UNSPECIFIED.,.F.,.F.,(4,1,1,4),(0.513473762730163,0.746551820444979,
0.901937192254856,1.05732256406473),.UNSPECIFIED.) ;
#618 = B_SPLINE_CURVE_WITH_KNOTS('',3,(#13286,#13287,#13288,#13289,#13290,
#13291),.UNSPECIFIED.,.F.,.F.,(4,1,1,4),(-1.05732256406473,-0.901937192254856,
-0.746551820444979,-0.513473762730163),.UNSPECIFIED.) ;
#619 = B_SPLINE_CURVE_WITH_KNOTS('',3,(#13296,#13297,#13298,#13299,#13300,
#13301),.UNSPECIFIED.,.F.,.F.,(4,1,1,4),(2.08427008952506,2.23965546133494,
2.39504083314481,2.62811889085963),.UNSPECIFIED.) ;
#620 = B_SPLINE_CURVE_WITH_KNOTS('',3,(#13305,#13306,#13307,#13308,#13309,
#13310),.UNSPECIFIED.,.F.,.F.,(4,1,1,4),(3.65506641631996,3.88814447403477,
4.04352984584465,4.19891521765453),.UNSPECIFIED.) ;
#621 = B_SPLINE_CURVE_WITH_KNOTS('',3,(#13314,#13315,#13316,#13317,#13318,
#13319),.UNSPECIFIED.,.F.,.F.,(4,1,1,4),(-1.05732256406473,-0.901937192254856,
-0.746551820444979,-0.513473762730164),.UNSPECIFIED.) ;
#622 = B_SPLINE_CURVE_WITH_KNOTS('',3,(#13365,#13366,#13367,#13368,#13369,
#13370),.UNSPECIFIED.,.F.,.F.,(4,1,1,4),(0.513473762730164,0.746551820444979,
0.901937192254856,1.05732256406473),.UNSPECIFIED.) ;
#623 = B_SPLINE_CURVE_WITH_KNOTS('',3,(#13408,#13409,#13410,#13411,#13412,
#13413),.UNSPECIFIED.,.F.,.F.,(4,1,1,4),(-4.19891521765453,-4.04352984584465,
-3.88814447403477,-3.65506641631996),.UNSPECIFIED.) ;
#624 = B_SPLINE_CURVE_WITH_KNOTS('',3,(#13451,#13452,#13453,#13454,#13455,
#13456),.UNSPECIFIED.,.F.,.F.,(4,1,1,4),(-2.62811889085963,-2.39504083314481,
-2.23965546133494,-2.08427008952506),.UNSPECIFIED.) ;
#625 = B_SPLINE_CURVE_WITH_KNOTS('',3,(#13724,#13725,#13726,#13727,#13728,
#13729,#13730,#13731,#13732,#13733),.UNSPECIFIED.,.F.,.F.,(4,3,3,4),(-4.09254174883839,
-3.97868581063554,-2.98401435797666,-2.06514013327809),.UNSPECIFIED.) ;
#626 = B_SPLINE_CURVE_WITH_KNOTS('',3,(#13736,#13737,#13738,#13739,#13740,
#13741,#13742),.UNSPECIFIED.,.F.,.F.,(4,3,4),(0.,0.994671452658877,1.11419103802963),
 .UNSPECIFIED.) ;
#627 = B_SPLINE_CURVE_WITH_KNOTS('',3,(#13747,#13748,#13749,#13750,#13751,
#13752,#13753,#13754,#13755,#13756,#13757,#13758,#13759,#13760,#13761,#13762,
#13763,#13764,#13765,#13766,#13767,#13768),.UNSPECIFIED.,.F.,.F.,(4,3,3,
3,3,3,3,4),(-10.375727056018,-9.94671452658885,-8.95204307392997,-7.95737162127108,
-6.96270016861219,-5.96802871595331,-4.97335726329442,-4.09254174883839),
 .UNSPECIFIED.) ;
#628 = B_SPLINE_CURVE_WITH_KNOTS('',3,(#13769,#13770,#13771,#13772,#13773,
#13774,#13775,#13776,#13777,#13778,#13779,#13780,#13781,#13782,#13783,#13784,
#13785,#13786,#13787,#13788,#13789,#13790),.UNSPECIFIED.,.F.,.F.,(4,3,3,
3,3,3,3,4),(1.11419103802963,1.98934290531777,2.98401435797665,3.97868581063554,
4.97335726329443,5.96802871595332,6.96270016861221,7.3973763452092),
 .UNSPECIFIED.) ;
#629 = B_SPLINE_CURVE_WITH_KNOTS('',3,(#13795,#13796,#13797,#13798,#13799,
#13800,#13801,#13802,#13803,#13804,#13805,#13806,#13807,#13808,#13809,#13810,
#13811,#13812,#13813,#13814,#13815,#13816),.UNSPECIFIED.,.F.,.F.,(4,3,3,
3,3,3,3,4),(-16.6589123631976,-15.9147432425422,-14.9200717898833,-13.9254003372244,
-12.9307288845655,-11.9360574319066,-10.9413859792477,-10.375727056018),
 .UNSPECIFIED.) ;
#630 = B_SPLINE_CURVE_WITH_KNOTS('',3,(#13817,#13818,#13819,#13820,#13821,
#13822,#13823,#13824,#13825,#13826,#13827,#13828,#13829,#13830,#13831,#13832,
#13833,#13834,#13835,#13836,#13837,#13838),.UNSPECIFIED.,.F.,.F.,(4,3,3,
3,3,3,3,4),(7.3973763452092,7.95737162127109,8.95204307392997,9.94671452658885,
10.9413859792477,11.9360574319066,12.9307288845655,13.6805616523888),
 .UNSPECIFIED.) ;
#631 = B_SPLINE_CURVE_WITH_KNOTS('',3,(#13843,#13844,#13845,#13846,#13847,
#13848,#13849,#13850,#13851,#13852,#13853,#13854,#13855,#13856,#13857,#13858,
#13859,#13860,#13861,#13862,#13863,#13864,#13865,#13866,#13867),
 .UNSPECIFIED.,.F.,.F.,(4,3,3,3,3,3,3,3,4),(-22.9420976703771,-22.8774434111544,
-21.8827719584955,-20.8881005058366,-19.8934290531777,-18.8987576005188,
-17.9040861478599,-16.9094146952011,-16.6589123631976),.UNSPECIFIED.) ;
#632 = B_SPLINE_CURVE_WITH_KNOTS('',3,(#13868,#13869,#13870,#13871,#13872,
#13873,#13874,#13875,#13876,#13877,#13878,#13879,#13880,#13881,#13882,#13883,
#13884,#13885,#13886,#13887,#13888,#13889,#13890,#13891,#13892),
 .UNSPECIFIED.,.F.,.F.,(4,3,3,3,3,3,3,3,4),(13.6805616523888,13.9254003372244,
14.9200717898833,15.9147432425422,16.909414695201,17.9040861478599,18.8987576005188,
19.8934290531777,19.9637469595684),.UNSPECIFIED.) ;
#633 = B_SPLINE_CURVE_WITH_KNOTS('',3,(#13897,#13898,#13899,#13900,#13901,
#13902,#13903,#13904,#13905,#13906,#13907,#13908,#13909,#13910,#13911,#13912,
#13913,#13914,#13915,#13916,#13917,#13918),.UNSPECIFIED.,.F.,.F.,(4,3,3,
3,3,3,3,4),(-29.2252829775567,-28.8454721271077,-27.8508006744488,-26.8561292217899,
-25.861457769131,-24.8667863164721,-23.8721148638132,-22.9420976703771),
 .UNSPECIFIED.) ;
#634 = B_SPLINE_CURVE_WITH_KNOTS('',3,(#13919,#13920,#13921,#13922,#13923,
#13924,#13925,#13926,#13927,#13928,#13929,#13930,#13931,#13932,#13933,#13934,
#13935,#13936,#13937,#13938,#13939,#13940),.UNSPECIFIED.,.F.,.F.,(4,3,3,
3,3,3,3,4),(19.9637469595684,20.8881005058366,21.8827719584955,22.8774434111544,
23.8721148638132,24.8667863164721,25.861457769131,26.246932266748),
 .UNSPECIFIED.) ;
#635 = B_SPLINE_CURVE_WITH_KNOTS('',3,(#13945,#13946,#13947,#13948,#13949,
#13950,#13951,#13952,#13953,#13954,#13955,#13956,#13957,#13958,#13959,#13960,
#13961,#13962,#13963,#13964,#13965,#13966),.UNSPECIFIED.,.F.,.F.,(4,3,3,
3,3,3,3,4),(-35.5084682847363,-34.813500843061,-33.8188293904021,-32.8241579377432,
-31.8294864850843,-30.8348150324254,-29.8401435797666,-29.2252829775567),
 .UNSPECIFIED.) ;
#636 = B_SPLINE_CURVE_WITH_KNOTS('',3,(#13967,#13968,#13969,#13970,#13971,
#13972,#13973,#13974,#13975,#13976,#13977,#13978,#13979,#13980,#13981,#13982,
#13983,#13984,#13985,#13986,#13987,#13988),.UNSPECIFIED.,.F.,.F.,(4,3,3,
3,3,3,3,4),(26.246932266748,26.8561292217899,27.8508006744488,28.8454721271077,
29.8401435797665,30.8348150324254,31.8294864850843,32.5301175739276),
 .UNSPECIFIED.) ;
#637 = B_SPLINE_CURVE_WITH_KNOTS('',3,(#13993,#13994,#13995,#13996,#13997,
#13998,#13999,#14000,#14001,#14002,#14003,#14004,#14005,#14006,#14007,#14008,
#14009,#14010,#14011,#14012,#14013,#14014,#14015,#14016,#14017),
 .UNSPECIFIED.,.F.,.F.,(4,3,3,3,3,3,3,3,4),(-41.7916535919159,-41.7762010116732,
-40.7815295590143,-39.7868581063554,-38.7921866536965,-37.7975152010376,
-36.8028437483788,-35.8081722957199,-35.5084682847363),.UNSPECIFIED.) ;
#638 = B_SPLINE_CURVE_WITH_KNOTS('',3,(#14018,#14019,#14020,#14021,#14022,
#14023,#14024,#14025,#14026,#14027,#14028,#14029,#14030,#14031,#14032,#14033,
#14034,#14035,#14036,#14037,#14038,#14039,#14040,#14041,#14042),
 .UNSPECIFIED.,.F.,.F.,(4,3,3,3,3,3,3,3,4),(32.5301175739276,32.8241579377432,
33.8188293904021,34.813500843061,35.8081722957199,36.8028437483787,37.7975152010376,
38.7921866536965,38.8133028811071),.UNSPECIFIED.) ;
#639 = B_SPLINE_CURVE_WITH_KNOTS('',3,(#14047,#14048,#14049,#14050,#14051,
#14052,#14053,#14054,#14055,#14056,#14057,#14058,#14059,#14060,#14061,#14062,
#14063,#14064,#14065,#14066,#14067,#14068),.UNSPECIFIED.,.F.,.F.,(4,3,3,
3,3,3,3,4),(-48.0748388990955,-47.7442297276265,-46.7495582749676,-45.7548868223087,
-44.7602153696498,-43.765543916991,-42.7708724643321,-41.7916535919159),
 .UNSPECIFIED.) ;
#640 = B_SPLINE_CURVE_WITH_KNOTS('',3,(#14069,#14070,#14071,#14072,#14073,
#14074,#14075,#14076,#14077,#14078,#14079,#14080,#14081,#14082,#14083,#14084,
#14085,#14086,#14087,#14088,#14089,#14090),.UNSPECIFIED.,.F.,.F.,(4,3,3,
3,3,3,3,4),(38.8133028811071,39.7868581063554,40.7815295590143,41.7762010116732,
42.7708724643321,43.7655439169909,44.7602153696498,45.0964881882867),
 .UNSPECIFIED.) ;
#641 = B_SPLINE_CURVE_WITH_KNOTS('',3,(#14095,#14096,#14097,#14098,#14099,
#14100,#14101,#14102,#14103,#14104,#14105,#14106,#14107,#14108,#14109,#14110,
#14111,#14112,#14113,#14114,#14115,#14116),.UNSPECIFIED.,.F.,.F.,(4,3,3,
3,3,3,3,4),(-54.3580242062751,-53.7122584435798,-52.7175869909209,-51.722915538262,
-50.7282440856032,-49.7335726329443,-48.7389011802854,-48.0748388990955),
 .UNSPECIFIED.) ;
#642 = B_SPLINE_CURVE_WITH_KNOTS('',3,(#14117,#14118,#14119,#14120,#14121,
#14122,#14123,#14124,#14125,#14126,#14127,#14128,#14129,#14130,#14131,#14132,
#14133,#14134,#14135,#14136,#14137,#14138),.UNSPECIFIED.,.F.,.F.,(4,3,3,
3,3,3,3,4),(45.0964881882867,45.7548868223087,46.7495582749676,47.7442297276265,
48.7389011802854,49.7335726329443,50.7282440856031,51.3796734954663),
 .UNSPECIFIED.) ;
#643 = B_SPLINE_CURVE_WITH_KNOTS('',3,(#14143,#14144,#14145,#14146,#14147,
#14148,#14149,#14150,#14151,#14152,#14153,#14154,#14155,#14156,#14157,#14158,
#14159,#14160,#14161,#14162,#14163,#14164),.UNSPECIFIED.,.F.,.F.,(4,3,3,
3,3,3,3,4),(-60.6412095134547,-59.6802871595331,-58.6856157068742,-57.6909442542154,
-56.6962728015565,-55.7016013488976,-54.7069298962387,-54.3580242062751),
 .UNSPECIFIED.) ;
#644 = B_SPLINE_CURVE_WITH_KNOTS('',3,(#14165,#14166,#14167,#14168,#14169,
#14170,#14171,#14172,#14173,#14174,#14175,#14176,#14177,#14178,#14179,#14180,
#14181,#14182,#14183,#14184,#14185,#14186),.UNSPECIFIED.,.F.,.F.,(4,3,3,
3,3,3,3,4),(51.3796734954663,51.722915538262,52.7175869909209,53.7122584435798,
54.7069298962387,55.7016013488976,56.6962728015565,57.6628588026459),
 .UNSPECIFIED.) ;
#645 = B_SPLINE_CURVE_WITH_KNOTS('',3,(#14191,#14192,#14193,#14194,#14195,
#14196,#14197,#14198,#14199,#14200,#14201,#14202,#14203,#14204,#14205,#14206,
#14207,#14208,#14209,#14210,#14211,#14212,#14213,#14214,#14215),
 .UNSPECIFIED.,.F.,.F.,(4,3,3,3,3,3,3,3,4),(-66.9243948206343,-66.6429873281453,
-65.6483158754864,-64.6536444228275,-63.6589729701686,-62.6643015175098,
-61.6696300648509,-60.674958612192,-60.6412095134547),.UNSPECIFIED.) ;
#646 = B_SPLINE_CURVE_WITH_KNOTS('',3,(#14216,#14217,#14218,#14219,#14220,
#14221,#14222,#14223,#14224,#14225,#14226,#14227,#14228,#14229,#14230,#14231,
#14232,#14233,#14234,#14235,#14236,#14237,#14238,#14239,#14240),
 .UNSPECIFIED.,.F.,.F.,(4,3,3,3,3,3,3,3,4),(57.6628588026459,57.6909442542153,
58.6856157068742,59.6802871595331,60.674958612192,61.6696300648509,62.6643015175098,
63.6589729701687,63.9460441098255),.UNSPECIFIED.) ;
#647 = B_SPLINE_CURVE_WITH_KNOTS('',3,(#14245,#14246,#14247,#14248,#14249,
#14250,#14251,#14252,#14253,#14254,#14255,#14256,#14257,#14258,#14259,#14260,
#14261,#14262,#14263,#14264,#14265,#14266),.UNSPECIFIED.,.F.,.F.,(4,3,3,
3,3,3,3,4),(-73.2075801278139,-72.6110160440986,-71.6163445914397,-70.6216731387808,
-69.627001686122,-68.6323302334631,-67.6376587808042,-66.9243948206343),
 .UNSPECIFIED.) ;
#648 = B_SPLINE_CURVE_WITH_KNOTS('',3,(#14267,#14268,#14269,#14270,#14271,
#14272,#14273,#14274,#14275,#14276,#14277,#14278,#14279,#14280,#14281,#14282,
#14283,#14284,#14285,#14286,#14287,#14288),.UNSPECIFIED.,.F.,.F.,(4,3,3,
3,3,3,3,4),(63.9460441098255,64.6536444228276,65.6483158754864,66.6429873281453,
67.6376587808042,68.6323302334631,69.627001686122,70.2292294170051),
 .UNSPECIFIED.) ;
#649 = B_SPLINE_CURVE_WITH_KNOTS('',3,(#14293,#14294,#14295,#14296,#14297,
#14298,#14299,#14300,#14301,#14302,#14303,#14304,#14305,#14306,#14307,#14308,
#14309,#14310,#14311,#14312,#14313,#14314),.UNSPECIFIED.,.F.,.F.,(4,3,3,
3,3,3,3,4),(-79.4907654349935,-78.5790447600519,-77.5843733073931,-76.5897018547342,
-75.5950304020753,-74.6003589494164,-73.6056874967575,-73.2075801278139),
 .UNSPECIFIED.) ;
#650 = B_SPLINE_CURVE_WITH_KNOTS('',3,(#14315,#14316,#14317,#14318,#14319,
#14320,#14321,#14322,#14323,#14324,#14325,#14326,#14327,#14328,#14329,#14330,
#14331,#14332,#14333,#14334,#14335,#14336),.UNSPECIFIED.,.F.,.F.,(4,3,3,
3,3,3,3,4),(70.2292294170051,70.6216731387808,71.6163445914397,72.6110160440986,
73.6056874967575,74.6003589494164,75.5950304020753,76.5124147241847),
 .UNSPECIFIED.) ;
#651 = B_SPLINE_CURVE_WITH_KNOTS('',3,(#14343,#14344,#14345,#14346,#14347,
#14348,#14349,#14350,#14351,#14352,#14353,#14354,#14355,#14356,#14357,#14358,
#14359,#14360,#14361,#14362,#14363,#14364),.UNSPECIFIED.,.F.,.F.,(4,3,3,
3,3,3,3,4),(-85.5417449286641,-84.5470734760052,-83.5524020233464,-82.5577305706875,
-81.5630591180286,-80.5683876653697,-79.5737162127108,-79.4907654349935),
 .UNSPECIFIED.) ;
#652 = B_SPLINE_CURVE_WITH_KNOTS('',3,(#14365,#14366,#14367,#14368,#14369,
#14370,#14371,#14372,#14373,#14374,#14375,#14376,#14377,#14378,#14379,#14380,
#14381,#14382,#14383,#14384,#14385,#14386,#14387,#14388,#14389),
 .UNSPECIFIED.,.F.,.F.,(4,3,3,3,3,3,3,3,4),(76.5124147241847,76.5897018547341,
77.584373307393,78.5790447600519,79.5737162127108,80.5683876653697,81.5630591180286,
82.5577305706875,82.7956000313643),.UNSPECIFIED.) ;
#653 = B_SPLINE_CURVE_WITH_KNOTS('',3,(#14395,#14396,#14397,#14398,#14399,
#14400,#14401,#14402),.UNSPECIFIED.,.F.,.F.,(4,1,1,1,1,4),(91.106186954104,
91.1891377318213,92.1838091844802,93.1784806371391,94.173152089798,95.0920263144966),
 .UNSPECIFIED.) ;
#654 = B_SPLINE_CURVE_WITH_KNOTS('',3,(#14405,#14406,#14407,#14408,#14409,
#14410),.UNSPECIFIED.,.F.,.F.,(4,1,1,4),(91.106186954104,91.862988946086,
92.8576603987449,93.8523318514037),.UNSPECIFIED.) ;
#655 = B_SPLINE_CURVE_WITH_KNOTS('',3,(#14415,#14416,#14417,#14418,#14419,
#14420,#14421,#14422,#14423,#14424),.UNSPECIFIED.,.F.,.F.,(4,1,1,1,1,1,
1,4),(84.8230016469244,85.221109015868,86.2157804685269,87.2104519211858,
88.2051233738447,89.1997948265036,90.1944662791624,91.106186954104),
 .UNSPECIFIED.) ;
#656 = B_SPLINE_CURVE_WITH_KNOTS('',3,(#14425,#14426,#14427,#14428,#14429,
#14430,#14431,#14432,#14433,#14434,#14435),.UNSPECIFIED.,.F.,.F.,(4,1,1,
1,1,1,1,1,4),(84.8230016469244,84.9002887774738,85.8949602301327,86.8896316827915,
87.8843031354504,88.8789745881093,89.8736460407682,90.8683174934271,91.106186954104),
 .UNSPECIFIED.) ;
#657 = B_SPLINE_CURVE_WITH_KNOTS('',3,(#14440,#14441,#14442,#14443,#14444,
#14445,#14446,#14447,#14448,#14449),.UNSPECIFIED.,.F.,.F.,(4,1,1,1,1,1,
1,4),(78.5398163397448,79.2530802999147,80.2477517525736,81.2424232052325,
82.2370946578914,83.2317661105503,84.2264375632091,84.8230016469244),
 .UNSPECIFIED.) ;
#658 = B_SPLINE_CURVE_WITH_KNOTS('',3,(#14450,#14451,#14452,#14453,#14454,
#14455,#14456,#14457,#14458,#14459),.UNSPECIFIED.,.F.,.F.,(4,1,1,1,1,1,
1,4),(78.5398163397448,78.9322600615205,79.9269315141794,80.9216029668382,
81.9162744194971,82.910945872156,83.9056173248149,84.8230016469244),
 .UNSPECIFIED.) ;
#659 = B_SPLINE_CURVE_WITH_KNOTS('',3,(#14464,#14465,#14466,#14467,#14468,
#14469,#14470,#14471,#14472,#14473,#14474),.UNSPECIFIED.,.F.,.F.,(4,1,1,
1,1,1,1,1,4),(72.2566310325652,72.2903801313025,73.2850515839614,74.2797230366203,
75.2743944892792,76.2690659419381,77.2637373945969,78.2584088472558,78.5398163397448),
 .UNSPECIFIED.) ;
#660 = B_SPLINE_CURVE_WITH_KNOTS('',3,(#14475,#14476,#14477,#14478,#14479,
#14480,#14481,#14482,#14483,#14484),.UNSPECIFIED.,.F.,.F.,(4,1,1,1,1,1,
1,4),(72.2566310325652,72.9642313455672,73.958902798226,74.9535742508849,
75.9482457035438,76.9429171562027,77.9375886088616,78.5398163397448),
 .UNSPECIFIED.) ;
#661 = B_SPLINE_CURVE_WITH_KNOTS('',3,(#14489,#14490,#14491,#14492,#14493,
#14494,#14495,#14496,#14497,#14498),.UNSPECIFIED.,.F.,.F.,(4,1,1,1,1,1,
1,4),(65.9734457253856,66.3223514153492,67.3170228680081,68.311694320667,
69.3063657733259,70.3010372259847,71.2957086786436,72.2566310325652),
 .UNSPECIFIED.) ;
#662 = B_SPLINE_CURVE_WITH_KNOTS('',3,(#14499,#14500,#14501,#14502,#14503,
#14504,#14505,#14506,#14507,#14508,#14509),.UNSPECIFIED.,.F.,.F.,(4,1,1,
1,1,1,1,1,4),(65.9734457253856,66.001531176955,66.9962026296138,67.9908740822727,
68.9855455349316,69.9802169875905,70.9748884402494,71.9695598929083,72.2566310325652),
 .UNSPECIFIED.) ;
#663 = B_SPLINE_CURVE_WITH_KNOTS('',3,(#14514,#14515,#14516,#14517,#14518,
#14519,#14520,#14521,#14522,#14523),.UNSPECIFIED.,.F.,.F.,(4,1,1,1,1,1,
1,4),(59.6902604182061,60.3543226993959,61.3489941520548,62.3436656047136,
63.3383370573725,64.3330085100314,65.3276799626903,65.9734457253856),
 .UNSPECIFIED.) ;
#664 = B_SPLINE_CURVE_WITH_KNOTS('',3,(#14524,#14525,#14526,#14527,#14528,
#14529,#14530,#14531,#14532,#14533),.UNSPECIFIED.,.F.,.F.,(4,1,1,1,1,1,
1,4),(59.690260418206,60.0335024610017,61.0281739136605,62.0228453663194,
63.0175168189783,64.0121882716372,65.0068597242961,65.9734457253856),
 .UNSPECIFIED.) ;
#665 = B_SPLINE_CURVE_WITH_KNOTS('',3,(#14538,#14539,#14540,#14541,#14542,
#14543,#14544,#14545,#14546,#14547),.UNSPECIFIED.,.F.,.F.,(4,1,1,1,1,1,
1,4),(53.4070751110265,54.3862939834426,55.3809654361015,56.3756368887603,
57.3703083414192,58.3649797940781,59.359651246737,59.6902604182061),
 .UNSPECIFIED.) ;
#666 = B_SPLINE_CURVE_WITH_KNOTS('',3,(#14548,#14549,#14550,#14551,#14552,
#14553,#14554,#14555,#14556,#14557),.UNSPECIFIED.,.F.,.F.,(4,1,1,1,1,1,
1,4),(53.4070751110265,54.0654737450483,55.0601451977072,56.0548166503661,
57.049488103025,58.0441595556839,59.0388310083428,59.690260418206),
 .UNSPECIFIED.) ;
#667 = B_SPLINE_CURVE_WITH_KNOTS('',3,(#14562,#14563,#14564,#14565,#14566,
#14567,#14568,#14569,#14570,#14571,#14572),.UNSPECIFIED.,.F.,.F.,(4,1,1,
1,1,1,1,1,4),(47.1238898038469,47.4235938148304,48.4182652674893,49.4129367201481,
50.407608172807,51.4022796254659,52.3969510781248,53.3916225307837,53.4070751110265),
 .UNSPECIFIED.) ;
#668 = B_SPLINE_CURVE_WITH_KNOTS('',3,(#14573,#14574,#14575,#14576,#14577,
#14578,#14579,#14580,#14581,#14582),.UNSPECIFIED.,.F.,.F.,(4,1,1,1,1,1,
1,4),(47.1238898038469,48.097445029095,49.0921164817539,50.0867879344128,
51.0814593870717,52.0761308397306,53.0708022923895,53.4070751110265),
 .UNSPECIFIED.) ;
#669 = B_SPLINE_CURVE_WITH_KNOTS('',3,(#14587,#14588,#14589,#14590,#14591,
#14592,#14593,#14594,#14595,#14596),.UNSPECIFIED.,.F.,.F.,(4,1,1,1,1,1,
1,4),(40.8407044966672,41.4555650988771,42.450236551536,43.4449080041948,
44.4395794568537,45.4342509095126,46.4289223621715,47.1238898038469),
 .UNSPECIFIED.) ;
#670 = B_SPLINE_CURVE_WITH_KNOTS('',3,(#14597,#14598,#14599,#14600,#14601,
#14602,#14603,#14604,#14605,#14606,#14607),.UNSPECIFIED.,.F.,.F.,(4,1,1,
1,1,1,1,1,4),(40.8407044966673,41.1347448604828,42.1294163131417,43.1240877658006,
44.1187592184595,45.1134306711184,46.1081021237773,47.1027735764361,47.1238898038469),
 .UNSPECIFIED.) ;
#671 = B_SPLINE_CURVE_WITH_KNOTS('',3,(#14612,#14613,#14614,#14615,#14616,
#14617,#14618,#14619,#14620,#14621),.UNSPECIFIED.,.F.,.F.,(4,1,1,1,1,1,
1,4),(34.5575191894877,35.4875363829238,36.4822078355826,37.4768792882415,
38.4715507409004,39.4662221935593,40.4608936462182,40.8407044966672),
 .UNSPECIFIED.) ;
#672 = B_SPLINE_CURVE_WITH_KNOTS('',3,(#14622,#14623,#14624,#14625,#14626,
#14627,#14628,#14629,#14630,#14631),.UNSPECIFIED.,.F.,.F.,(4,1,1,1,1,1,
1,4),(34.5575191894877,35.1667161445295,36.1613875971884,37.1560590498473,
38.1507305025062,39.1454019551651,40.1400734078239,40.8407044966673),
 .UNSPECIFIED.) ;
#673 = B_SPLINE_CURVE_WITH_KNOTS('',3,(#14636,#14637,#14638,#14639,#14640,
#14641,#14642,#14643,#14644,#14645,#14646),.UNSPECIFIED.,.F.,.F.,(4,1,1,
1,1,1,1,1,4),(28.2743338823081,28.5248362143116,29.5195076669704,30.5141791196293,
31.5088505722882,32.5035220249471,33.498193477606,34.4928649302649,34.5575191894877),
 .UNSPECIFIED.) ;
#674 = B_SPLINE_CURVE_WITH_KNOTS('',3,(#14647,#14648,#14649,#14650,#14651,
#14652,#14653,#14654,#14655,#14656),.UNSPECIFIED.,.F.,.F.,(4,1,1,1,1,1,
1,4),(28.2743338823081,29.1986874285762,30.1933588812351,31.188030333894,
32.1827017865529,33.1773732392118,34.1720446918706,34.5575191894877),
 .UNSPECIFIED.) ;
#675 = B_SPLINE_CURVE_WITH_KNOTS('',3,(#14661,#14662,#14663,#14664,#14665,
#14666,#14667,#14668,#14669,#14670),.UNSPECIFIED.,.F.,.F.,(4,1,1,1,1,1,
1,4),(21.9911485751285,22.5568074983582,23.5514789510171,24.546150403676,
25.5408218563349,26.5354933089938,27.5301647616527,28.2743338823081),
 .UNSPECIFIED.) ;
#676 = B_SPLINE_CURVE_WITH_KNOTS('',3,(#14671,#14672,#14673,#14674,#14675,
#14676,#14677,#14678,#14679,#14680,#14681),.UNSPECIFIED.,.F.,.F.,(4,1,1,
1,1,1,1,1,4),(21.9911485751285,22.235987259964,23.2306587126229,24.2253301652818,
25.2200016179407,26.2146730705996,27.2093445232584,28.2040159759173,28.2743338823081),
 .UNSPECIFIED.) ;
#677 = B_SPLINE_CURVE_WITH_KNOTS('',3,(#14686,#14687,#14688,#14689,#14690,
#14691,#14692,#14693,#14694,#14695),.UNSPECIFIED.,.F.,.F.,(4,1,1,1,1,1,
1,4),(15.7079632679489,16.5887787824049,17.5834502350638,18.5781216877227,
19.5727931403816,20.5674645930405,21.5621360456994,21.9911485751285),
 .UNSPECIFIED.) ;
#678 = B_SPLINE_CURVE_WITH_KNOTS('',3,(#14696,#14697,#14698,#14699,#14700,
#14701,#14702,#14703,#14704,#14705),.UNSPECIFIED.,.F.,.F.,(4,1,1,1,1,1,
1,4),(15.7079632679489,16.2679585440107,17.2626299966696,18.2573014493285,
19.2519729019874,20.2466443546463,21.2413158073051,21.9911485751285),
 .UNSPECIFIED.) ;
#679 = B_SPLINE_CURVE_WITH_KNOTS('',3,(#14707,#14708,#14709,#14710,#14711,
#14712,#14713,#14714,#14715,#14716,#14717,#14718,#14719,#14720,#14721,#14722,
#14723,#14724,#14725,#14726,#14727,#14728,#14729,#14730,#14731,#14732,#14733,
#14734,#14735,#14736,#14737,#14738,#14739,#14740,#14741,#14742,#14743,#14744,
#14745,#14746,#14747,#14748,#14749,#14750,#14751,#14752,#14753,#14754,#14755,
#14756,#14757,#14758,#14759,#14760,#14761,#14762,#14763,#14764,#14765,#14766,
#14767,#14768,#14769,#14770,#14771,#14772,#14773,#14774,#14775,#14776,#14777,
#14778,#14779,#14780,#14781,#14782,#14783,#14784,#14785,#14786,#14787,#14788,
#14789,#14790,#14791,#14792,#14793,#14794),.UNSPECIFIED.,.F.,.F.,(4,3,3,
3,3,3,3,3,3,3,3,3,3,3,3,3,3,3,3,3,3,3,3,3,3,3,3,3,3,4),(-0.366397579005862,
-0.354400153901985,-0.336404777063956,-0.325308561006329,-0.321425114196814,
-0.302615912560535,-0.288115700084732,-0.282369417309185,-0.278676253632104,
-0.259267773940829,-0.239450435117437,-0.226241379526605,-0.219675125726992,
-0.215147934128903,-0.211940642009688,-0.191508203259365,-0.186614212754108,
-0.166896800453023,-0.156170429838319,-0.146894080558608,-0.143763204851242,
-0.123283757624856,-0.102374268823611,-0.0813088122791208,-0.0759017170823301,
-0.0722481990532672,-0.0506067082153849,-0.0289141439014962,-0.00768477071724965,
0.),.UNSPECIFIED.) ;
#680 = B_SPLINE_CURVE_WITH_KNOTS('',3,(#14797,#14798,#14799,#14800,#14801,
#14802,#14803,#14804,#14805,#14806,#14807,#14808,#14809,#14810,#14811,#14812,
#14813,#14814,#14815,#14816,#14817,#14818,#14819,#14820,#14821,#14822,#14823,
#14824,#14825,#14826,#14827,#14828,#14829,#14830,#14831,#14832,#14833,#14834,
#14835,#14836,#14837,#14838,#14839,#14840,#14841,#14842,#14843,#14844,#14845,
#14846,#14847,#14848,#14849,#14850,#14851,#14852,#14853,#14854,#14855,#14856,
#14857,#14858,#14859,#14860,#14861,#14862,#14863,#14864,#14865,#14866,#14867,
#14868,#14869,#14870,#14871,#14872,#14873,#14874,#14875,#14876,#14877,#14878,
#14879,#14880,#14881,#14882,#14883,#14884),.UNSPECIFIED.,.F.,.F.,(4,3,3,
3,3,3,3,3,3,3,3,3,3,3,3,3,3,3,3,3,3,3,3,3,3,3,3,3,3,4),(-0.364629307890639,
-0.349849466571909,-0.328248388013126,-0.317414684226437,-0.313033716262076,
-0.291718379827004,-0.275966596123573,-0.26769149370129,-0.263902447125792,
-0.26027159190815,-0.239539956910309,-0.219314376336061,-0.205911809801935,
-0.194395827041001,-0.191067917075939,-0.171483017238108,-0.165704110199559,
-0.144723738467068,-0.135144345214647,-0.126400867612846,-0.123094476845862,
-0.103639598986686,-0.0842677857508656,-0.0652966313372813,-0.0619884758863919,
-0.0584739564360926,-0.0398922435233024,-0.0216481816196747,-0.00398472010826969,
0.),.UNSPECIFIED.) ;
#681 = B_SPLINE_CURVE_WITH_KNOTS('',3,(#15241,#15242,#15243,#15244),
 .UNSPECIFIED.,.F.,.F.,(4,4),(82.7956000313643,83.4766047953861),
 .UNSPECIFIED.) ;
#682 = B_SPLINE_CURVE_WITH_KNOTS('',3,(#15246,#15247,#15248,#15249,#15250,
#15251,#15252,#15253,#15254,#15255,#15256,#15257,#15258,#15259,#15260,#15261,
#15262,#15263,#15264,#15265,#15266,#15267,#15268,#15269,#15270,#15271,#15272,
#15273,#15274,#15275,#15276,#15277,#15278,#15279,#15280,#15281,#15282,#15283,
#15284,#15285,#15286,#15287,#15288,#15289,#15290,#15291,#15292,#15293,#15294,
#15295,#15296,#15297,#15298,#15299,#15300,#15301,#15302,#15303,#15304,#15305,
#15306,#15307,#15308,#15309,#15310,#15311,#15312,#15313,#15314,#15315,#15316,
#15317,#15318,#15319,#15320,#15321,#15322,#15323,#15324,#15325,#15326,#15327,
#15328,#15329,#15330,#15331,#15332,#15333),.UNSPECIFIED.,.F.,.F.,(4,3,3,
3,3,3,3,3,3,3,3,3,3,3,3,3,3,3,3,3,3,3,3,3,3,3,3,3,3,4),(-0.366397579005832,
-0.35440015390196,-0.336404774950202,-0.325308556551589,-0.321425108353319,
-0.302615905227926,-0.288115693668699,-0.282369381594845,-0.278676239117541,
-0.259267757976344,-0.239450419326581,-0.226241367683462,-0.219675101906396,
-0.215147723883162,-0.211940603206927,-0.19150816459754,-0.186614212754105,
-0.166896799655008,-0.15617042880848,-0.146894076502295,-0.14376319718546,
-0.123283748791081,-0.102374258882692,-0.0813088023174796,-0.0759017003095587,
-0.0722481957683859,-0.0506067042383249,-0.0289141405258821,-0.00768477040946941,
0.),.UNSPECIFIED.) ;
#683 = B_SPLINE_CURVE_WITH_KNOTS('',3,(#15334,#15335,#15336,#15337,#15338,
#15339,#15340,#15341,#15342),.UNSPECIFIED.,.F.,.F.,(4,1,1,1,1,1,4),(10.3757270560177,
11.2946012807163,12.2892727333752,13.2839441860341,14.2786156386929,15.2732870913518,
15.7079632679489),.UNSPECIFIED.) ;
#684 = B_SPLINE_CURVE_WITH_KNOTS('',3,(#15347,#15348,#15349,#15350,#15351,
#15352,#15353,#15354,#15355,#15356,#15357,#15358,#15359,#15360,#15361,#15362,
#15363,#15364,#15365,#15366,#15367,#15368,#15369,#15370,#15371,#15372,#15373,
#15374,#15375,#15376,#15377,#15378,#15379,#15380,#15381,#15382,#15383,#15384,
#15385,#15386,#15387,#15388,#15389,#15390,#15391,#15392,#15393,#15394,#15395,
#15396,#15397,#15398,#15399,#15400,#15401,#15402,#15403,#15404,#15405,#15406,
#15407,#15408,#15409,#15410,#15411,#15412,#15413,#15414,#15415,#15416,#15417,
#15418,#15419,#15420,#15421,#15422,#15423,#15424,#15425,#15426,#15427,#15428,
#15429,#15430,#15431,#15432,#15433,#15434),.UNSPECIFIED.,.F.,.F.,(4,3,3,
3,3,3,3,3,3,3,3,3,3,3,3,3,3,3,3,3,3,3,3,3,3,3,3,3,3,4),(-0.364629307890559,
-0.349849466571842,-0.328248388005598,-0.317414684778512,-0.313033717426747,
-0.291718381011116,-0.275966597159668,-0.267691495007892,-0.263902448445838,
-0.260271592580404,-0.239539957901017,-0.219314379339481,-0.205911812054494,
-0.194395830861808,-0.191067922191916,-0.171483024299037,-0.165704110199532,
-0.144723710840863,-0.135144314569244,-0.126400708769428,-0.123094450949365,
-0.103639573299063,-0.0842677588660923,-0.0652966020700892,-0.0619884278297192,
-0.0584739451235707,-0.0398922301008105,-0.0216481651996582,-0.00398470002455966,
0.),.UNSPECIFIED.) ;
#685 = B_SPLINE_CURVE_WITH_KNOTS('',3,(#15438,#15439,#15440,#15441,#15442,
#15443,#15444,#15445),.UNSPECIFIED.,.F.,.F.,(4,1,1,1,1,4),(11.6154215191105,
12.6100929717694,13.6047644244283,14.5994358770872,15.594107329746,15.7079632679489),
 .UNSPECIFIED.) ;
#686 = FACE_BOUND('',#1506,.T.) ;
#687 = FACE_BOUND('',#1511,.T.) ;
#688 = FACE_BOUND('',#1536,.T.) ;
#689 = FACE_BOUND('',#1540,.T.) ;
#690 = FACE_BOUND('',#1542,.T.) ;
#691 = FACE_BOUND('',#1573,.T.) ;
#692 = FACE_BOUND('',#1585,.T.) ;
#693 = FACE_BOUND('',#1586,.T.) ;
#694 = FACE_BOUND('',#1587,.T.) ;
#695 = FACE_BOUND('',#1588,.T.) ;
#696 = FACE_BOUND('',#1589,.T.) ;
#697 = FACE_BOUND('',#1590,.T.) ;
#698 = FACE_BOUND('',#1591,.T.) ;
#699 = FACE_BOUND('',#1592,.T.) ;
#700 = FACE_BOUND('',#1691,.T.) ;
#701 = FACE_BOUND('',#1693,.T.) ;
#702 = FACE_BOUND('',#1709,.T.) ;
#703 = FACE_BOUND('',#1711,.T.) ;
#704 = FACE_BOUND('',#1713,.T.) ;
#705 = FACE_BOUND('',#1715,.T.) ;
#706 = FACE_BOUND('',#1725,.T.) ;
#707 = FACE_BOUND('',#1731,.T.) ;
#708 = FACE_BOUND('',#1734,.T.) ;
#709 = FACE_BOUND('',#1737,.T.) ;
#710 = FACE_BOUND('',#1740,.T.) ;
#711 = FACE_BOUND('',#1743,.T.) ;
#712 = FACE_BOUND('',#1746,.T.) ;
#713 = FACE_BOUND('',#1749,.T.) ;
#714 = FACE_BOUND('',#1750,.T.) ;
#715 = FACE_BOUND('',#1751,.T.) ;
#716 = FACE_BOUND('',#1752,.T.) ;
#717 = FACE_BOUND('',#1753,.T.) ;
#718 = FACE_BOUND('',#1759,.T.) ;
#719 = FACE_BOUND('',#1778,.T.) ;
#720 = FACE_BOUND('',#1779,.T.) ;
#721 = FACE_BOUND('',#1780,.T.) ;
#722 = FACE_BOUND('',#1781,.T.) ;
#723 = FACE_BOUND('',#1783,.T.) ;
#724 = FACE_BOUND('',#1785,.T.) ;
#725 = FACE_BOUND('',#1786,.T.) ;
#726 = FACE_BOUND('',#1787,.T.) ;
#727 = FACE_BOUND('',#1788,.T.) ;
#728 = FACE_BOUND('',#1790,.T.) ;
#729 = FACE_BOUND('',#1827,.T.) ;
#730 = FACE_BOUND('',#1942,.T.) ;
#731 = FACE_BOUND('',#1970,.T.) ;
#732 = FACE_BOUND('',#1973,.T.) ;
#733 = FACE_BOUND('',#1985,.T.) ;
#734 = FACE_BOUND('',#1986,.T.) ;
#735 = FACE_BOUND('',#1994,.T.) ;
#736 = FACE_BOUND('',#1995,.T.) ;
#737 = PLANE('',#8271) ;
#738 = PLANE('',#8280) ;
#739 = PLANE('',#8283) ;
#740 = PLANE('',#8286) ;
#741 = PLANE('',#8287) ;
#742 = PLANE('',#8290) ;
#743 = PLANE('',#8292) ;
#744 = PLANE('',#8293) ;
#745 = PLANE('',#8335) ;
#746 = PLANE('',#8340) ;
#747 = PLANE('',#8346) ;
#748 = PLANE('',#8348) ;
#749 = PLANE('',#8349) ;
#750 = PLANE('',#8351) ;
#751 = PLANE('',#8352) ;
#752 = PLANE('',#8354) ;
#753 = PLANE('',#8355) ;
#754 = PLANE('',#8357) ;
#755 = PLANE('',#8387) ;
#756 = PLANE('',#8388) ;
#757 = PLANE('',#8389) ;
#758 = PLANE('',#8390) ;
#759 = PLANE('',#8391) ;
#760 = PLANE('',#8392) ;
#761 = PLANE('',#8393) ;
#762 = PLANE('',#8394) ;
#763 = PLANE('',#8395) ;
#764 = PLANE('',#8396) ;
#765 = PLANE('',#8397) ;
#766 = PLANE('',#8398) ;
#767 = PLANE('',#8399) ;
#768 = PLANE('',#8400) ;
#769 = PLANE('',#8401) ;
#770 = PLANE('',#8402) ;
#771 = PLANE('',#8403) ;
#772 = PLANE('',#8404) ;
#773 = PLANE('',#8405) ;
#774 = PLANE('',#8406) ;
#775 = PLANE('',#8407) ;
#776 = PLANE('',#8408) ;
#777 = PLANE('',#8409) ;
#778 = PLANE('',#8410) ;
#779 = PLANE('',#8411) ;
#780 = PLANE('',#8412) ;
#781 = PLANE('',#8413) ;
#782 = PLANE('',#8414) ;
#783 = PLANE('',#8415) ;
#784 = PLANE('',#8416) ;
#785 = PLANE('',#8417) ;
#786 = PLANE('',#8418) ;
#787 = PLANE('',#8419) ;
#788 = PLANE('',#8420) ;
#789 = PLANE('',#8421) ;
#790 = PLANE('',#8422) ;
#791 = PLANE('',#8423) ;
#792 = PLANE('',#8424) ;
#793 = PLANE('',#8425) ;
#794 = PLANE('',#8426) ;
#795 = PLANE('',#8427) ;
#796 = PLANE('',#8428) ;
#797 = PLANE('',#8429) ;
#798 = PLANE('',#8430) ;
#799 = PLANE('',#8431) ;
#800 = PLANE('',#8432) ;
#801 = PLANE('',#8433) ;
#802 = PLANE('',#8434) ;
#803 = PLANE('',#8438) ;
#804 = PLANE('',#8440) ;
#805 = PLANE('',#8475) ;
#806 = PLANE('',#8477) ;
#807 = PLANE('',#8479) ;
#808 = PLANE('',#8481) ;
#809 = PLANE('',#8503) ;
#810 = PLANE('',#8517) ;
#811 = PLANE('',#8520) ;
#812 = PLANE('',#8525) ;
#813 = PLANE('',#8529) ;
#814 = PLANE('',#8534) ;
#815 = PLANE('',#8538) ;
#816 = PLANE('',#8541) ;
#817 = PLANE('',#8550) ;
#818 = PLANE('',#8553) ;
#819 = PLANE('',#8554) ;
#820 = PLANE('',#8557) ;
#821 = PLANE('',#8558) ;
#822 = PLANE('',#8561) ;
#823 = PLANE('',#8562) ;
#824 = PLANE('',#8565) ;
#825 = PLANE('',#8566) ;
#826 = PLANE('',#8569) ;
#827 = PLANE('',#8570) ;
#828 = PLANE('',#8573) ;
#829 = PLANE('',#8574) ;
#830 = PLANE('',#8577) ;
#831 = PLANE('',#8578) ;
#832 = PLANE('',#8581) ;
#833 = PLANE('',#8582) ;
#834 = PLANE('',#8588) ;
#835 = PLANE('',#8592) ;
#836 = PLANE('',#8627) ;
#837 = PLANE('',#8629) ;
#838 = PLANE('',#8639) ;
#839 = PLANE('',#8643) ;
#840 = PLANE('',#8644) ;
#841 = PLANE('',#8645) ;
#842 = PLANE('',#8647) ;
#843 = PLANE('',#8722) ;
#844 = PLANE('',#8723) ;
#845 = PLANE('',#8724) ;
#846 = PLANE('',#8725) ;
#847 = PLANE('',#8726) ;
#848 = PLANE('',#8727) ;
#849 = PLANE('',#8728) ;
#850 = PLANE('',#8729) ;
#851 = PLANE('',#8730) ;
#852 = PLANE('',#8731) ;
#853 = PLANE('',#8732) ;
#854 = PLANE('',#8733) ;
#855 = PLANE('',#8734) ;
#856 = PLANE('',#8735) ;
#857 = PLANE('',#8736) ;
#858 = PLANE('',#8737) ;
#859 = PLANE('',#8738) ;
#860 = PLANE('',#8739) ;
#861 = PLANE('',#8740) ;
#862 = PLANE('',#8741) ;
#863 = PLANE('',#8742) ;
#864 = PLANE('',#8743) ;
#865 = PLANE('',#8744) ;
#866 = PLANE('',#8745) ;
#867 = PLANE('',#8746) ;
#868 = PLANE('',#8747) ;
#869 = PLANE('',#8748) ;
#870 = PLANE('',#8749) ;
#871 = PLANE('',#8750) ;
#872 = PLANE('',#8751) ;
#873 = PLANE('',#8752) ;
#874 = PLANE('',#8753) ;
#875 = PLANE('',#8754) ;
#876 = PLANE('',#8755) ;
#877 = PLANE('',#8756) ;
#878 = PLANE('',#8757) ;
#879 = PLANE('',#8758) ;
#880 = PLANE('',#8759) ;
#881 = PLANE('',#8760) ;
#882 = PLANE('',#8761) ;
#883 = PLANE('',#8762) ;
#884 = PLANE('',#8763) ;
#885 = PLANE('',#8764) ;
#886 = PLANE('',#8765) ;
#887 = PLANE('',#8766) ;
#888 = PLANE('',#8767) ;
#889 = PLANE('',#8768) ;
#890 = PLANE('',#8769) ;
#891 = PLANE('',#8770) ;
#892 = PLANE('',#8771) ;
#893 = PLANE('',#8772) ;
#894 = PLANE('',#8773) ;
#895 = PLANE('',#8774) ;
#896 = PLANE('',#8775) ;
#897 = PLANE('',#8776) ;
#898 = PLANE('',#8777) ;
#899 = PLANE('',#8778) ;
#900 = PLANE('',#8779) ;
#901 = PLANE('',#8780) ;
#902 = PLANE('',#8781) ;
#903 = PLANE('',#8782) ;
#904 = PLANE('',#8783) ;
#905 = PLANE('',#8784) ;
#906 = PLANE('',#8785) ;
#907 = PLANE('',#8786) ;
#908 = PLANE('',#8787) ;
#909 = PLANE('',#8788) ;
#910 = PLANE('',#8789) ;
#911 = PLANE('',#8790) ;
#912 = PLANE('',#8791) ;
#913 = PLANE('',#8792) ;
#914 = PLANE('',#8793) ;
#915 = PLANE('',#8794) ;
#916 = PLANE('',#8795) ;
#917 = PLANE('',#8796) ;
#918 = PLANE('',#8797) ;
#919 = PLANE('',#8798) ;
#920 = PLANE('',#8799) ;
#921 = PLANE('',#8800) ;
#922 = PLANE('',#8801) ;
#923 = PLANE('',#8802) ;
#924 = PLANE('',#8803) ;
#925 = PLANE('',#8804) ;
#926 = PLANE('',#8805) ;
#927 = PLANE('',#8806) ;
#928 = PLANE('',#8807) ;
#929 = PLANE('',#8808) ;
#930 = PLANE('',#8809) ;
#931 = PLANE('',#8810) ;
#932 = PLANE('',#8811) ;
#933 = PLANE('',#8812) ;
#934 = PLANE('',#8813) ;
#935 = PLANE('',#8814) ;
#936 = PLANE('',#8815) ;
#937 = PLANE('',#8816) ;
#938 = PLANE('',#8817) ;
#939 = PLANE('',#8818) ;
#940 = PLANE('',#8819) ;
#941 = PLANE('',#8820) ;
#942 = PLANE('',#8821) ;
#943 = PLANE('',#8822) ;
#944 = PLANE('',#8823) ;
#945 = PLANE('',#8824) ;
#946 = PLANE('',#8825) ;
#947 = PLANE('',#8826) ;
#948 = PLANE('',#8831) ;
#949 = PLANE('',#8852) ;
#950 = PLANE('',#8853) ;
#951 = PLANE('',#8854) ;
#952 = PLANE('',#8855) ;
#953 = PLANE('',#8856) ;
#954 = PLANE('',#8857) ;
#955 = PLANE('',#8858) ;
#956 = PLANE('',#8859) ;
#957 = PLANE('',#8860) ;
#958 = PLANE('',#8861) ;
#959 = PLANE('',#8863) ;
#960 = PLANE('',#8865) ;
#961 = PLANE('',#8867) ;
#962 = PLANE('',#8869) ;
#963 = PLANE('',#8871) ;
#964 = PLANE('',#8874) ;
#965 = PLANE('',#8875) ;
#966 = PLANE('',#8876) ;
#967 = PLANE('',#8878) ;
#968 = PLANE('',#8883) ;
#969 = PLANE('',#8900) ;
#970 = PLANE('',#8901) ;
#971 = PLANE('',#8902) ;
#972 = PLANE('',#8903) ;
#973 = PLANE('',#8909) ;
#974 = PLANE('',#8910) ;
#975 = PLANE('',#8913) ;
#976 = PLANE('',#8916) ;
#977 = CYLINDRICAL_SURFACE('',#8268,4.05) ;
#978 = CYLINDRICAL_SURFACE('',#8277,4.05) ;
#979 = CYLINDRICAL_SURFACE('',#8295,1.65) ;
#980 = CYLINDRICAL_SURFACE('',#8298,1.65) ;
#981 = CYLINDRICAL_SURFACE('',#8301,1.65) ;
#982 = CYLINDRICAL_SURFACE('',#8304,1.65) ;
#983 = CYLINDRICAL_SURFACE('',#8319,8.) ;
#984 = CYLINDRICAL_SURFACE('',#8321,8.) ;
#985 = CYLINDRICAL_SURFACE('',#8323,8.) ;
#986 = CYLINDRICAL_SURFACE('',#8325,8.) ;
#987 = CYLINDRICAL_SURFACE('',#8339,6.) ;
#988 = CYLINDRICAL_SURFACE('',#8342,6.) ;
#989 = CYLINDRICAL_SURFACE('',#8358,15.5) ;
#990 = CYLINDRICAL_SURFACE('',#8435,15.1) ;
#991 = CYLINDRICAL_SURFACE('',#8441,15.5) ;
#992 = CYLINDRICAL_SURFACE('',#8455,4.) ;
#993 = CYLINDRICAL_SURFACE('',#8461,4.) ;
#994 = CYLINDRICAL_SURFACE('',#8467,4.) ;
#995 = CYLINDRICAL_SURFACE('',#8473,4.) ;
#996 = CYLINDRICAL_SURFACE('',#8483,2.25) ;
#997 = CYLINDRICAL_SURFACE('',#8485,2.25) ;
#998 = CYLINDRICAL_SURFACE('',#8487,2.25) ;
#999 = CYLINDRICAL_SURFACE('',#8489,2.25) ;
#1000 = CYLINDRICAL_SURFACE('',#8491,1.65) ;
#1001 = CYLINDRICAL_SURFACE('',#8494,1.65) ;
#1002 = CYLINDRICAL_SURFACE('',#8497,1.65) ;
#1003 = CYLINDRICAL_SURFACE('',#8500,1.65) ;
#1004 = CYLINDRICAL_SURFACE('',#8509,8.6) ;
#1005 = CYLINDRICAL_SURFACE('',#8511,8.6) ;
#1006 = CYLINDRICAL_SURFACE('',#8513,8.6) ;
#1007 = CYLINDRICAL_SURFACE('',#8515,8.6) ;
#1008 = CYLINDRICAL_SURFACE('',#8519,15.5) ;
#1009 = CYLINDRICAL_SURFACE('',#8523,12.6) ;
#1010 = CYLINDRICAL_SURFACE('',#8527,12.) ;
#1011 = CYLINDRICAL_SURFACE('',#8532,12.6) ;
#1012 = CYLINDRICAL_SURFACE('',#8536,12.) ;
#1013 = CYLINDRICAL_SURFACE('',#8539,12.) ;
#1014 = CYLINDRICAL_SURFACE('',#8545,25.5) ;
#1015 = CYLINDRICAL_SURFACE('',#8551,12.) ;
#1016 = CYLINDRICAL_SURFACE('',#8585,8.15) ;
#1017 = CYLINDRICAL_SURFACE('',#8590,8.5) ;
#1018 = CYLINDRICAL_SURFACE('',#8597,1.954) ;
#1019 = CYLINDRICAL_SURFACE('',#8599,1.954) ;
#1020 = CYLINDRICAL_SURFACE('',#8600,1.954) ;
#1021 = CYLINDRICAL_SURFACE('',#8601,1.954) ;
#1022 = CYLINDRICAL_SURFACE('',#8602,1.954) ;
#1023 = CYLINDRICAL_SURFACE('',#8603,1.954) ;
#1024 = CYLINDRICAL_SURFACE('',#8604,1.954) ;
#1025 = CYLINDRICAL_SURFACE('',#8605,1.954) ;
#1026 = CYLINDRICAL_SURFACE('',#8606,1.954) ;
#1027 = CYLINDRICAL_SURFACE('',#8607,1.954) ;
#1028 = CYLINDRICAL_SURFACE('',#8608,1.954) ;
#1029 = CYLINDRICAL_SURFACE('',#8609,1.954) ;
#1030 = CYLINDRICAL_SURFACE('',#8610,1.954) ;
#1031 = CYLINDRICAL_SURFACE('',#8611,1.954) ;
#1032 = CYLINDRICAL_SURFACE('',#8613,1.5555) ;
#1033 = CYLINDRICAL_SURFACE('',#8615,1.5555) ;
#1034 = CYLINDRICAL_SURFACE('',#8616,1.5555) ;
#1035 = CYLINDRICAL_SURFACE('',#8617,1.5555) ;
#1036 = CYLINDRICAL_SURFACE('',#8618,1.5555) ;
#1037 = CYLINDRICAL_SURFACE('',#8619,1.5555) ;
#1038 = CYLINDRICAL_SURFACE('',#8620,1.5555) ;
#1039 = CYLINDRICAL_SURFACE('',#8621,1.5555) ;
#1040 = CYLINDRICAL_SURFACE('',#8622,1.5555) ;
#1041 = CYLINDRICAL_SURFACE('',#8623,1.5555) ;
#1042 = CYLINDRICAL_SURFACE('',#8624,1.5555) ;
#1043 = CYLINDRICAL_SURFACE('',#8625,1.5555) ;
#1044 = CYLINDRICAL_SURFACE('',#8626,1.5555) ;
#1045 = CYLINDRICAL_SURFACE('',#8633,1.5555) ;
#1046 = CYLINDRICAL_SURFACE('',#8637,1.954) ;
#1047 = CYLINDRICAL_SURFACE('',#8648,3.5) ;
#1048 = CYLINDRICAL_SURFACE('',#8840,1.68205080756887) ;
#1049 = CYLINDRICAL_SURFACE('',#8842,1.68205080756887) ;
#1050 = CYLINDRICAL_SURFACE('',#8844,1.68205080756887) ;
#1051 = CYLINDRICAL_SURFACE('',#8846,1.68205080756887) ;
#1052 = CYLINDRICAL_SURFACE('',#8848,1.68205080756887) ;
#1053 = CYLINDRICAL_SURFACE('',#8850,1.68205080756887) ;
#1054 = CYLINDRICAL_SURFACE('',#8881,12.) ;
#1055 = CYLINDRICAL_SURFACE('',#8887,8.05) ;
#1056 = CYLINDRICAL_SURFACE('',#8893,8.05) ;
#1057 = CYLINDRICAL_SURFACE('',#8897,0.85) ;
#1058 = CYLINDRICAL_SURFACE('',#8907,0.85) ;
#1059 = CYLINDRICAL_SURFACE('',#8911,10.2) ;
#1060 = CYLINDRICAL_SURFACE('',#8914,12.55) ;
#1061 = FACE_OUTER_BOUND('',#1503,.T.) ;
#1062 = FACE_OUTER_BOUND('',#1504,.T.) ;
#1063 = FACE_OUTER_BOUND('',#1505,.T.) ;
#1064 = FACE_OUTER_BOUND('',#1507,.T.) ;
#1065 = FACE_OUTER_BOUND('',#1508,.T.) ;
#1066 = FACE_OUTER_BOUND('',#1509,.T.) ;
#1067 = FACE_OUTER_BOUND('',#1510,.T.) ;
#1068 = FACE_OUTER_BOUND('',#1512,.T.) ;
#1069 = FACE_OUTER_BOUND('',#1513,.T.) ;
#1070 = FACE_OUTER_BOUND('',#1514,.T.) ;
#1071 = FACE_OUTER_BOUND('',#1515,.T.) ;
#1072 = FACE_OUTER_BOUND('',#1516,.T.) ;
#1073 = FACE_OUTER_BOUND('',#1517,.T.) ;
#1074 = FACE_OUTER_BOUND('',#1518,.T.) ;
#1075 = FACE_OUTER_BOUND('',#1519,.T.) ;
#1076 = FACE_OUTER_BOUND('',#1520,.T.) ;
#1077 = FACE_OUTER_BOUND('',#1521,.T.) ;
#1078 = FACE_OUTER_BOUND('',#1522,.T.) ;
#1079 = FACE_OUTER_BOUND('',#1523,.T.) ;
#1080 = FACE_OUTER_BOUND('',#1524,.T.) ;
#1081 = FACE_OUTER_BOUND('',#1525,.T.) ;
#1082 = FACE_OUTER_BOUND('',#1526,.T.) ;
#1083 = FACE_OUTER_BOUND('',#1527,.T.) ;
#1084 = FACE_OUTER_BOUND('',#1528,.T.) ;
#1085 = FACE_OUTER_BOUND('',#1529,.T.) ;
#1086 = FACE_OUTER_BOUND('',#1530,.T.) ;
#1087 = FACE_OUTER_BOUND('',#1531,.T.) ;
#1088 = FACE_OUTER_BOUND('',#1532,.T.) ;
#1089 = FACE_OUTER_BOUND('',#1533,.T.) ;
#1090 = FACE_OUTER_BOUND('',#1534,.T.) ;
#1091 = FACE_OUTER_BOUND('',#1535,.T.) ;
#1092 = FACE_OUTER_BOUND('',#1537,.T.) ;
#1093 = FACE_OUTER_BOUND('',#1538,.T.) ;
#1094 = FACE_OUTER_BOUND('',#1539,.T.) ;
#1095 = FACE_OUTER_BOUND('',#1541,.T.) ;
#1096 = FACE_OUTER_BOUND('',#1543,.T.) ;
#1097 = FACE_OUTER_BOUND('',#1544,.T.) ;
#1098 = FACE_OUTER_BOUND('',#1545,.T.) ;
#1099 = FACE_OUTER_BOUND('',#1546,.T.) ;
#1100 = FACE_OUTER_BOUND('',#1547,.T.) ;
#1101 = FACE_OUTER_BOUND('',#1548,.T.) ;
#1102 = FACE_OUTER_BOUND('',#1549,.T.) ;
#1103 = FACE_OUTER_BOUND('',#1550,.T.) ;
#1104 = FACE_OUTER_BOUND('',#1551,.T.) ;
#1105 = FACE_OUTER_BOUND('',#1552,.T.) ;
#1106 = FACE_OUTER_BOUND('',#1553,.T.) ;
#1107 = FACE_OUTER_BOUND('',#1554,.T.) ;
#1108 = FACE_OUTER_BOUND('',#1555,.T.) ;
#1109 = FACE_OUTER_BOUND('',#1556,.T.) ;
#1110 = FACE_OUTER_BOUND('',#1557,.T.) ;
#1111 = FACE_OUTER_BOUND('',#1558,.T.) ;
#1112 = FACE_OUTER_BOUND('',#1559,.T.) ;
#1113 = FACE_OUTER_BOUND('',#1560,.T.) ;
#1114 = FACE_OUTER_BOUND('',#1561,.T.) ;
#1115 = FACE_OUTER_BOUND('',#1562,.T.) ;
#1116 = FACE_OUTER_BOUND('',#1563,.T.) ;
#1117 = FACE_OUTER_BOUND('',#1564,.T.) ;
#1118 = FACE_OUTER_BOUND('',#1565,.T.) ;
#1119 = FACE_OUTER_BOUND('',#1566,.T.) ;
#1120 = FACE_OUTER_BOUND('',#1567,.T.) ;
#1121 = FACE_OUTER_BOUND('',#1568,.T.) ;
#1122 = FACE_OUTER_BOUND('',#1569,.T.) ;
#1123 = FACE_OUTER_BOUND('',#1570,.T.) ;
#1124 = FACE_OUTER_BOUND('',#1571,.T.) ;
#1125 = FACE_OUTER_BOUND('',#1572,.T.) ;
#1126 = FACE_OUTER_BOUND('',#1574,.T.) ;
#1127 = FACE_OUTER_BOUND('',#1575,.T.) ;
#1128 = FACE_OUTER_BOUND('',#1576,.T.) ;
#1129 = FACE_OUTER_BOUND('',#1577,.T.) ;
#1130 = FACE_OUTER_BOUND('',#1578,.T.) ;
#1131 = FACE_OUTER_BOUND('',#1579,.T.) ;
#1132 = FACE_OUTER_BOUND('',#1580,.T.) ;
#1133 = FACE_OUTER_BOUND('',#1581,.T.) ;
#1134 = FACE_OUTER_BOUND('',#1582,.T.) ;
#1135 = FACE_OUTER_BOUND('',#1583,.T.) ;
#1136 = FACE_OUTER_BOUND('',#1584,.T.) ;
#1137 = FACE_OUTER_BOUND('',#1593,.T.) ;
#1138 = FACE_OUTER_BOUND('',#1594,.T.) ;
#1139 = FACE_OUTER_BOUND('',#1595,.T.) ;
#1140 = FACE_OUTER_BOUND('',#1596,.T.) ;
#1141 = FACE_OUTER_BOUND('',#1597,.T.) ;
#1142 = FACE_OUTER_BOUND('',#1598,.T.) ;
#1143 = FACE_OUTER_BOUND('',#1599,.T.) ;
#1144 = FACE_OUTER_BOUND('',#1600,.T.) ;
#1145 = FACE_OUTER_BOUND('',#1601,.T.) ;
#1146 = FACE_OUTER_BOUND('',#1602,.T.) ;
#1147 = FACE_OUTER_BOUND('',#1603,.T.) ;
#1148 = FACE_OUTER_BOUND('',#1604,.T.) ;
#1149 = FACE_OUTER_BOUND('',#1605,.T.) ;
#1150 = FACE_OUTER_BOUND('',#1606,.T.) ;
#1151 = FACE_OUTER_BOUND('',#1607,.T.) ;
#1152 = FACE_OUTER_BOUND('',#1608,.T.) ;
#1153 = FACE_OUTER_BOUND('',#1609,.T.) ;
#1154 = FACE_OUTER_BOUND('',#1610,.T.) ;
#1155 = FACE_OUTER_BOUND('',#1611,.T.) ;
#1156 = FACE_OUTER_BOUND('',#1612,.T.) ;
#1157 = FACE_OUTER_BOUND('',#1613,.T.) ;
#1158 = FACE_OUTER_BOUND('',#1614,.T.) ;
#1159 = FACE_OUTER_BOUND('',#1615,.T.) ;
#1160 = FACE_OUTER_BOUND('',#1616,.T.) ;
#1161 = FACE_OUTER_BOUND('',#1617,.T.) ;
#1162 = FACE_OUTER_BOUND('',#1618,.T.) ;
#1163 = FACE_OUTER_BOUND('',#1619,.T.) ;
#1164 = FACE_OUTER_BOUND('',#1620,.T.) ;
#1165 = FACE_OUTER_BOUND('',#1621,.T.) ;
#1166 = FACE_OUTER_BOUND('',#1622,.T.) ;
#1167 = FACE_OUTER_BOUND('',#1623,.T.) ;
#1168 = FACE_OUTER_BOUND('',#1624,.T.) ;
#1169 = FACE_OUTER_BOUND('',#1625,.T.) ;
#1170 = FACE_OUTER_BOUND('',#1626,.T.) ;
#1171 = FACE_OUTER_BOUND('',#1627,.T.) ;
#1172 = FACE_OUTER_BOUND('',#1628,.T.) ;
#1173 = FACE_OUTER_BOUND('',#1629,.T.) ;
#1174 = FACE_OUTER_BOUND('',#1630,.T.) ;
#1175 = FACE_OUTER_BOUND('',#1631,.T.) ;
#1176 = FACE_OUTER_BOUND('',#1632,.T.) ;
#1177 = FACE_OUTER_BOUND('',#1633,.T.) ;
#1178 = FACE_OUTER_BOUND('',#1634,.T.) ;
#1179 = FACE_OUTER_BOUND('',#1635,.T.) ;
#1180 = FACE_OUTER_BOUND('',#1636,.T.) ;
#1181 = FACE_OUTER_BOUND('',#1637,.T.) ;
#1182 = FACE_OUTER_BOUND('',#1638,.T.) ;
#1183 = FACE_OUTER_BOUND('',#1639,.T.) ;
#1184 = FACE_OUTER_BOUND('',#1640,.T.) ;
#1185 = FACE_OUTER_BOUND('',#1641,.T.) ;
#1186 = FACE_OUTER_BOUND('',#1642,.T.) ;
#1187 = FACE_OUTER_BOUND('',#1643,.T.) ;
#1188 = FACE_OUTER_BOUND('',#1644,.T.) ;
#1189 = FACE_OUTER_BOUND('',#1645,.T.) ;
#1190 = FACE_OUTER_BOUND('',#1646,.T.) ;
#1191 = FACE_OUTER_BOUND('',#1647,.T.) ;
#1192 = FACE_OUTER_BOUND('',#1648,.T.) ;
#1193 = FACE_OUTER_BOUND('',#1649,.T.) ;
#1194 = FACE_OUTER_BOUND('',#1650,.T.) ;
#1195 = FACE_OUTER_BOUND('',#1651,.T.) ;
#1196 = FACE_OUTER_BOUND('',#1652,.T.) ;
#1197 = FACE_OUTER_BOUND('',#1653,.T.) ;
#1198 = FACE_OUTER_BOUND('',#1654,.T.) ;
#1199 = FACE_OUTER_BOUND('',#1655,.T.) ;
#1200 = FACE_OUTER_BOUND('',#1656,.T.) ;
#1201 = FACE_OUTER_BOUND('',#1657,.T.) ;
#1202 = FACE_OUTER_BOUND('',#1658,.T.) ;
#1203 = FACE_OUTER_BOUND('',#1659,.T.) ;
#1204 = FACE_OUTER_BOUND('',#1660,.T.) ;
#1205 = FACE_OUTER_BOUND('',#1661,.T.) ;
#1206 = FACE_OUTER_BOUND('',#1662,.T.) ;
#1207 = FACE_OUTER_BOUND('',#1663,.T.) ;
#1208 = FACE_OUTER_BOUND('',#1664,.T.) ;
#1209 = FACE_OUTER_BOUND('',#1665,.T.) ;
#1210 = FACE_OUTER_BOUND('',#1666,.T.) ;
#1211 = FACE_OUTER_BOUND('',#1667,.T.) ;
#1212 = FACE_OUTER_BOUND('',#1668,.T.) ;
#1213 = FACE_OUTER_BOUND('',#1669,.T.) ;
#1214 = FACE_OUTER_BOUND('',#1670,.T.) ;
#1215 = FACE_OUTER_BOUND('',#1671,.T.) ;
#1216 = FACE_OUTER_BOUND('',#1672,.T.) ;
#1217 = FACE_OUTER_BOUND('',#1673,.T.) ;
#1218 = FACE_OUTER_BOUND('',#1674,.T.) ;
#1219 = FACE_OUTER_BOUND('',#1675,.T.) ;
#1220 = FACE_OUTER_BOUND('',#1676,.T.) ;
#1221 = FACE_OUTER_BOUND('',#1677,.T.) ;
#1222 = FACE_OUTER_BOUND('',#1678,.T.) ;
#1223 = FACE_OUTER_BOUND('',#1679,.T.) ;
#1224 = FACE_OUTER_BOUND('',#1680,.T.) ;
#1225 = FACE_OUTER_BOUND('',#1681,.T.) ;
#1226 = FACE_OUTER_BOUND('',#1682,.T.) ;
#1227 = FACE_OUTER_BOUND('',#1683,.T.) ;
#1228 = FACE_OUTER_BOUND('',#1684,.T.) ;
#1229 = FACE_OUTER_BOUND('',#1685,.T.) ;
#1230 = FACE_OUTER_BOUND('',#1686,.T.) ;
#1231 = FACE_OUTER_BOUND('',#1687,.T.) ;
#1232 = FACE_OUTER_BOUND('',#1688,.T.) ;
#1233 = FACE_OUTER_BOUND('',#1689,.T.) ;
#1234 = FACE_OUTER_BOUND('',#1690,.T.) ;
#1235 = FACE_OUTER_BOUND('',#1692,.T.) ;
#1236 = FACE_OUTER_BOUND('',#1694,.T.) ;
#1237 = FACE_OUTER_BOUND('',#1695,.T.) ;
#1238 = FACE_OUTER_BOUND('',#1696,.T.) ;
#1239 = FACE_OUTER_BOUND('',#1697,.T.) ;
#1240 = FACE_OUTER_BOUND('',#1698,.T.) ;
#1241 = FACE_OUTER_BOUND('',#1699,.T.) ;
#1242 = FACE_OUTER_BOUND('',#1700,.T.) ;
#1243 = FACE_OUTER_BOUND('',#1701,.T.) ;
#1244 = FACE_OUTER_BOUND('',#1702,.T.) ;
#1245 = FACE_OUTER_BOUND('',#1703,.T.) ;
#1246 = FACE_OUTER_BOUND('',#1704,.T.) ;
#1247 = FACE_OUTER_BOUND('',#1705,.T.) ;
#1248 = FACE_OUTER_BOUND('',#1706,.T.) ;
#1249 = FACE_OUTER_BOUND('',#1707,.T.) ;
#1250 = FACE_OUTER_BOUND('',#1708,.T.) ;
#1251 = FACE_OUTER_BOUND('',#1710,.T.) ;
#1252 = FACE_OUTER_BOUND('',#1712,.T.) ;
#1253 = FACE_OUTER_BOUND('',#1714,.T.) ;
#1254 = FACE_OUTER_BOUND('',#1716,.T.) ;
#1255 = FACE_OUTER_BOUND('',#1717,.T.) ;
#1256 = FACE_OUTER_BOUND('',#1718,.T.) ;
#1257 = FACE_OUTER_BOUND('',#1719,.T.) ;
#1258 = FACE_OUTER_BOUND('',#1720,.T.) ;
#1259 = FACE_OUTER_BOUND('',#1721,.T.) ;
#1260 = FACE_OUTER_BOUND('',#1722,.T.) ;
#1261 = FACE_OUTER_BOUND('',#1723,.T.) ;
#1262 = FACE_OUTER_BOUND('',#1724,.T.) ;
#1263 = FACE_OUTER_BOUND('',#1726,.T.) ;
#1264 = FACE_OUTER_BOUND('',#1727,.T.) ;
#1265 = FACE_OUTER_BOUND('',#1728,.T.) ;
#1266 = FACE_OUTER_BOUND('',#1729,.T.) ;
#1267 = FACE_OUTER_BOUND('',#1730,.T.) ;
#1268 = FACE_OUTER_BOUND('',#1732,.T.) ;
#1269 = FACE_OUTER_BOUND('',#1733,.T.) ;
#1270 = FACE_OUTER_BOUND('',#1735,.T.) ;
#1271 = FACE_OUTER_BOUND('',#1736,.T.) ;
#1272 = FACE_OUTER_BOUND('',#1738,.T.) ;
#1273 = FACE_OUTER_BOUND('',#1739,.T.) ;
#1274 = FACE_OUTER_BOUND('',#1741,.T.) ;
#1275 = FACE_OUTER_BOUND('',#1742,.T.) ;
#1276 = FACE_OUTER_BOUND('',#1744,.T.) ;
#1277 = FACE_OUTER_BOUND('',#1745,.T.) ;
#1278 = FACE_OUTER_BOUND('',#1747,.T.) ;
#1279 = FACE_OUTER_BOUND('',#1748,.T.) ;
#1280 = FACE_OUTER_BOUND('',#1754,.T.) ;
#1281 = FACE_OUTER_BOUND('',#1755,.T.) ;
#1282 = FACE_OUTER_BOUND('',#1756,.T.) ;
#1283 = FACE_OUTER_BOUND('',#1757,.T.) ;
#1284 = FACE_OUTER_BOUND('',#1758,.T.) ;
#1285 = FACE_OUTER_BOUND('',#1760,.T.) ;
#1286 = FACE_OUTER_BOUND('',#1761,.T.) ;
#1287 = FACE_OUTER_BOUND('',#1762,.T.) ;
#1288 = FACE_OUTER_BOUND('',#1763,.T.) ;
#1289 = FACE_OUTER_BOUND('',#1764,.T.) ;
#1290 = FACE_OUTER_BOUND('',#1765,.T.) ;
#1291 = FACE_OUTER_BOUND('',#1766,.T.) ;
#1292 = FACE_OUTER_BOUND('',#1767,.T.) ;
#1293 = FACE_OUTER_BOUND('',#1768,.T.) ;
#1294 = FACE_OUTER_BOUND('',#1769,.T.) ;
#1295 = FACE_OUTER_BOUND('',#1770,.T.) ;
#1296 = FACE_OUTER_BOUND('',#1771,.T.) ;
#1297 = FACE_OUTER_BOUND('',#1772,.T.) ;
#1298 = FACE_OUTER_BOUND('',#1773,.T.) ;
#1299 = FACE_OUTER_BOUND('',#1774,.T.) ;
#1300 = FACE_OUTER_BOUND('',#1775,.T.) ;
#1301 = FACE_OUTER_BOUND('',#1776,.T.) ;
#1302 = FACE_OUTER_BOUND('',#1777,.T.) ;
#1303 = FACE_OUTER_BOUND('',#1782,.T.) ;
#1304 = FACE_OUTER_BOUND('',#1784,.T.) ;
#1305 = FACE_OUTER_BOUND('',#1789,.T.) ;
#1306 = FACE_OUTER_BOUND('',#1791,.T.) ;
#1307 = FACE_OUTER_BOUND('',#1792,.T.) ;
#1308 = FACE_OUTER_BOUND('',#1793,.T.) ;
#1309 = FACE_OUTER_BOUND('',#1794,.T.) ;
#1310 = FACE_OUTER_BOUND('',#1795,.T.) ;
#1311 = FACE_OUTER_BOUND('',#1796,.T.) ;
#1312 = FACE_OUTER_BOUND('',#1797,.T.) ;
#1313 = FACE_OUTER_BOUND('',#1798,.T.) ;
#1314 = FACE_OUTER_BOUND('',#1799,.T.) ;
#1315 = FACE_OUTER_BOUND('',#1800,.T.) ;
#1316 = FACE_OUTER_BOUND('',#1801,.T.) ;
#1317 = FACE_OUTER_BOUND('',#1802,.T.) ;
#1318 = FACE_OUTER_BOUND('',#1803,.T.) ;
#1319 = FACE_OUTER_BOUND('',#1804,.T.) ;
#1320 = FACE_OUTER_BOUND('',#1805,.T.) ;
#1321 = FACE_OUTER_BOUND('',#1806,.T.) ;
#1322 = FACE_OUTER_BOUND('',#1807,.T.) ;
#1323 = FACE_OUTER_BOUND('',#1808,.T.) ;
#1324 = FACE_OUTER_BOUND('',#1809,.T.) ;
#1325 = FACE_OUTER_BOUND('',#1810,.T.) ;
#1326 = FACE_OUTER_BOUND('',#1811,.T.) ;
#1327 = FACE_OUTER_BOUND('',#1812,.T.) ;
#1328 = FACE_OUTER_BOUND('',#1813,.T.) ;
#1329 = FACE_OUTER_BOUND('',#1814,.T.) ;
#1330 = FACE_OUTER_BOUND('',#1815,.T.) ;
#1331 = FACE_OUTER_BOUND('',#1816,.T.) ;
#1332 = FACE_OUTER_BOUND('',#1817,.T.) ;
#1333 = FACE_OUTER_BOUND('',#1818,.T.) ;
#1334 = FACE_OUTER_BOUND('',#1819,.T.) ;
#1335 = FACE_OUTER_BOUND('',#1820,.T.) ;
#1336 = FACE_OUTER_BOUND('',#1821,.T.) ;
#1337 = FACE_OUTER_BOUND('',#1822,.T.) ;
#1338 = FACE_OUTER_BOUND('',#1823,.T.) ;
#1339 = FACE_OUTER_BOUND('',#1824,.T.) ;
#1340 = FACE_OUTER_BOUND('',#1825,.T.) ;
#1341 = FACE_OUTER_BOUND('',#1826,.T.) ;
#1342 = FACE_OUTER_BOUND('',#1828,.T.) ;
#1343 = FACE_OUTER_BOUND('',#1829,.T.) ;
#1344 = FACE_OUTER_BOUND('',#1830,.T.) ;
#1345 = FACE_OUTER_BOUND('',#1831,.T.) ;
#1346 = FACE_OUTER_BOUND('',#1832,.T.) ;
#1347 = FACE_OUTER_BOUND('',#1833,.T.) ;
#1348 = FACE_OUTER_BOUND('',#1834,.T.) ;
#1349 = FACE_OUTER_BOUND('',#1835,.T.) ;
#1350 = FACE_OUTER_BOUND('',#1836,.T.) ;
#1351 = FACE_OUTER_BOUND('',#1837,.T.) ;
#1352 = FACE_OUTER_BOUND('',#1838,.T.) ;
#1353 = FACE_OUTER_BOUND('',#1839,.T.) ;
#1354 = FACE_OUTER_BOUND('',#1840,.T.) ;
#1355 = FACE_OUTER_BOUND('',#1841,.T.) ;
#1356 = FACE_OUTER_BOUND('',#1842,.T.) ;
#1357 = FACE_OUTER_BOUND('',#1843,.T.) ;
#1358 = FACE_OUTER_BOUND('',#1844,.T.) ;
#1359 = FACE_OUTER_BOUND('',#1845,.T.) ;
#1360 = FACE_OUTER_BOUND('',#1846,.T.) ;
#1361 = FACE_OUTER_BOUND('',#1847,.T.) ;
#1362 = FACE_OUTER_BOUND('',#1848,.T.) ;
#1363 = FACE_OUTER_BOUND('',#1849,.T.) ;
#1364 = FACE_OUTER_BOUND('',#1850,.T.) ;
#1365 = FACE_OUTER_BOUND('',#1851,.T.) ;
#1366 = FACE_OUTER_BOUND('',#1852,.T.) ;
#1367 = FACE_OUTER_BOUND('',#1853,.T.) ;
#1368 = FACE_OUTER_BOUND('',#1854,.T.) ;
#1369 = FACE_OUTER_BOUND('',#1855,.T.) ;
#1370 = FACE_OUTER_BOUND('',#1856,.T.) ;
#1371 = FACE_OUTER_BOUND('',#1857,.T.) ;
#1372 = FACE_OUTER_BOUND('',#1858,.T.) ;
#1373 = FACE_OUTER_BOUND('',#1859,.T.) ;
#1374 = FACE_OUTER_BOUND('',#1860,.T.) ;
#1375 = FACE_OUTER_BOUND('',#1861,.T.) ;
#1376 = FACE_OUTER_BOUND('',#1862,.T.) ;
#1377 = FACE_OUTER_BOUND('',#1863,.T.) ;
#1378 = FACE_OUTER_BOUND('',#1864,.T.) ;
#1379 = FACE_OUTER_BOUND('',#1865,.T.) ;
#1380 = FACE_OUTER_BOUND('',#1866,.T.) ;
#1381 = FACE_OUTER_BOUND('',#1867,.T.) ;
#1382 = FACE_OUTER_BOUND('',#1868,.T.) ;
#1383 = FACE_OUTER_BOUND('',#1869,.T.) ;
#1384 = FACE_OUTER_BOUND('',#1870,.T.) ;
#1385 = FACE_OUTER_BOUND('',#1871,.T.) ;
#1386 = FACE_OUTER_BOUND('',#1872,.T.) ;
#1387 = FACE_OUTER_BOUND('',#1873,.T.) ;
#1388 = FACE_OUTER_BOUND('',#1874,.T.) ;
#1389 = FACE_OUTER_BOUND('',#1875,.T.) ;
#1390 = FACE_OUTER_BOUND('',#1876,.T.) ;
#1391 = FACE_OUTER_BOUND('',#1877,.T.) ;
#1392 = FACE_OUTER_BOUND('',#1878,.T.) ;
#1393 = FACE_OUTER_BOUND('',#1879,.T.) ;
#1394 = FACE_OUTER_BOUND('',#1880,.T.) ;
#1395 = FACE_OUTER_BOUND('',#1881,.T.) ;
#1396 = FACE_OUTER_BOUND('',#1882,.T.) ;
#1397 = FACE_OUTER_BOUND('',#1883,.T.) ;
#1398 = FACE_OUTER_BOUND('',#1884,.T.) ;
#1399 = FACE_OUTER_BOUND('',#1885,.T.) ;
#1400 = FACE_OUTER_BOUND('',#1886,.T.) ;
#1401 = FACE_OUTER_BOUND('',#1887,.T.) ;
#1402 = FACE_OUTER_BOUND('',#1888,.T.) ;
#1403 = FACE_OUTER_BOUND('',#1889,.T.) ;
#1404 = FACE_OUTER_BOUND('',#1890,.T.) ;
#1405 = FACE_OUTER_BOUND('',#1891,.T.) ;
#1406 = FACE_OUTER_BOUND('',#1892,.T.) ;
#1407 = FACE_OUTER_BOUND('',#1893,.T.) ;
#1408 = FACE_OUTER_BOUND('',#1894,.T.) ;
#1409 = FACE_OUTER_BOUND('',#1895,.T.) ;
#1410 = FACE_OUTER_BOUND('',#1896,.T.) ;
#1411 = FACE_OUTER_BOUND('',#1897,.T.) ;
#1412 = FACE_OUTER_BOUND('',#1898,.T.) ;
#1413 = FACE_OUTER_BOUND('',#1899,.T.) ;
#1414 = FACE_OUTER_BOUND('',#1900,.T.) ;
#1415 = FACE_OUTER_BOUND('',#1901,.T.) ;
#1416 = FACE_OUTER_BOUND('',#1902,.T.) ;
#1417 = FACE_OUTER_BOUND('',#1903,.T.) ;
#1418 = FACE_OUTER_BOUND('',#1904,.T.) ;
#1419 = FACE_OUTER_BOUND('',#1905,.T.) ;
#1420 = FACE_OUTER_BOUND('',#1906,.T.) ;
#1421 = FACE_OUTER_BOUND('',#1907,.T.) ;
#1422 = FACE_OUTER_BOUND('',#1908,.T.) ;
#1423 = FACE_OUTER_BOUND('',#1909,.T.) ;
#1424 = FACE_OUTER_BOUND('',#1910,.T.) ;
#1425 = FACE_OUTER_BOUND('',#1911,.T.) ;
#1426 = FACE_OUTER_BOUND('',#1912,.T.) ;
#1427 = FACE_OUTER_BOUND('',#1913,.T.) ;
#1428 = FACE_OUTER_BOUND('',#1914,.T.) ;
#1429 = FACE_OUTER_BOUND('',#1915,.T.) ;
#1430 = FACE_OUTER_BOUND('',#1916,.T.) ;
#1431 = FACE_OUTER_BOUND('',#1917,.T.) ;
#1432 = FACE_OUTER_BOUND('',#1918,.T.) ;
#1433 = FACE_OUTER_BOUND('',#1919,.T.) ;
#1434 = FACE_OUTER_BOUND('',#1920,.T.) ;
#1435 = FACE_OUTER_BOUND('',#1921,.T.) ;
#1436 = FACE_OUTER_BOUND('',#1922,.T.) ;
#1437 = FACE_OUTER_BOUND('',#1923,.T.) ;
#1438 = FACE_OUTER_BOUND('',#1924,.T.) ;
#1439 = FACE_OUTER_BOUND('',#1925,.T.) ;
#1440 = FACE_OUTER_BOUND('',#1926,.T.) ;
#1441 = FACE_OUTER_BOUND('',#1927,.T.) ;
#1442 = FACE_OUTER_BOUND('',#1928,.T.) ;
#1443 = FACE_OUTER_BOUND('',#1929,.T.) ;
#1444 = FACE_OUTER_BOUND('',#1930,.T.) ;
#1445 = FACE_OUTER_BOUND('',#1931,.T.) ;
#1446 = FACE_OUTER_BOUND('',#1932,.T.) ;
#1447 = FACE_OUTER_BOUND('',#1933,.T.) ;
#1448 = FACE_OUTER_BOUND('',#1934,.T.) ;
#1449 = FACE_OUTER_BOUND('',#1935,.T.) ;
#1450 = FACE_OUTER_BOUND('',#1936,.T.) ;
#1451 = FACE_OUTER_BOUND('',#1937,.T.) ;
#1452 = FACE_OUTER_BOUND('',#1938,.T.) ;
#1453 = FACE_OUTER_BOUND('',#1939,.T.) ;
#1454 = FACE_OUTER_BOUND('',#1940,.T.) ;
#1455 = FACE_OUTER_BOUND('',#1941,.T.) ;
#1456 = FACE_OUTER_BOUND('',#1943,.T.) ;
#1457 = FACE_OUTER_BOUND('',#1944,.T.) ;
#1458 = FACE_OUTER_BOUND('',#1945,.T.) ;
#1459 = FACE_OUTER_BOUND('',#1946,.T.) ;
#1460 = FACE_OUTER_BOUND('',#1947,.T.) ;
#1461 = FACE_OUTER_BOUND('',#1948,.T.) ;
#1462 = FACE_OUTER_BOUND('',#1949,.T.) ;
#1463 = FACE_OUTER_BOUND('',#1950,.T.) ;
#1464 = FACE_OUTER_BOUND('',#1951,.T.) ;
#1465 = FACE_OUTER_BOUND('',#1952,.T.) ;
#1466 = FACE_OUTER_BOUND('',#1953,.T.) ;
#1467 = FACE_OUTER_BOUND('',#1954,.T.) ;
#1468 = FACE_OUTER_BOUND('',#1955,.T.) ;
#1469 = FACE_OUTER_BOUND('',#1956,.T.) ;
#1470 = FACE_OUTER_BOUND('',#1957,.T.) ;
#1471 = FACE_OUTER_BOUND('',#1958,.T.) ;
#1472 = FACE_OUTER_BOUND('',#1959,.T.) ;
#1473 = FACE_OUTER_BOUND('',#1960,.T.) ;
#1474 = FACE_OUTER_BOUND('',#1961,.T.) ;
#1475 = FACE_OUTER_BOUND('',#1962,.T.) ;
#1476 = FACE_OUTER_BOUND('',#1963,.T.) ;
#1477 = FACE_OUTER_BOUND('',#1964,.T.) ;
#1478 = FACE_OUTER_BOUND('',#1965,.T.) ;
#1479 = FACE_OUTER_BOUND('',#1966,.T.) ;
#1480 = FACE_OUTER_BOUND('',#1967,.T.) ;
#1481 = FACE_OUTER_BOUND('',#1968,.T.) ;
#1482 = FACE_OUTER_BOUND('',#1969,.T.) ;
#1483 = FACE_OUTER_BOUND('',#1971,.T.) ;
#1484 = FACE_OUTER_BOUND('',#1972,.T.) ;
#1485 = FACE_OUTER_BOUND('',#1974,.T.) ;
#1486 = FACE_OUTER_BOUND('',#1975,.T.) ;
#1487 = FACE_OUTER_BOUND('',#1976,.T.) ;
#1488 = FACE_OUTER_BOUND('',#1977,.T.) ;
#1489 = FACE_OUTER_BOUND('',#1978,.T.) ;
#1490 = FACE_OUTER_BOUND('',#1979,.T.) ;
#1491 = FACE_OUTER_BOUND('',#1980,.T.) ;
#1492 = FACE_OUTER_BOUND('',#1981,.T.) ;
#1493 = FACE_OUTER_BOUND('',#1982,.T.) ;
#1494 = FACE_OUTER_BOUND('',#1983,.T.) ;
#1495 = FACE_OUTER_BOUND('',#1984,.T.) ;
#1496 = FACE_OUTER_BOUND('',#1987,.T.) ;
#1497 = FACE_OUTER_BOUND('',#1988,.T.) ;
#1498 = FACE_OUTER_BOUND('',#1989,.T.) ;
#1499 = FACE_OUTER_BOUND('',#1990,.T.) ;
#1500 = FACE_OUTER_BOUND('',#1991,.T.) ;
#1501 = FACE_OUTER_BOUND('',#1992,.T.) ;
#1502 = FACE_OUTER_BOUND('',#1993,.T.) ;
#1503 = EDGE_LOOP('',(#5351,#5352,#5353,#5354)) ;
#1504 = EDGE_LOOP('',(#5355,#5356,#5357,#5358,#5359)) ;
#1505 = EDGE_LOOP('',(#5360)) ;
#1506 = EDGE_LOOP('',(#5361)) ;
#1507 = EDGE_LOOP('',(#5362,#5363,#5364,#5365)) ;
#1508 = EDGE_LOOP('',(#5366,#5367,#5368,#5369)) ;
#1509 = EDGE_LOOP('',(#5370,#5371,#5372,#5373,#5374)) ;
#1510 = EDGE_LOOP('',(#5375)) ;
#1511 = EDGE_LOOP('',(#5376)) ;
#1512 = EDGE_LOOP('',(#5377,#5378,#5379,#5380)) ;
#1513 = EDGE_LOOP('',(#5381,#5382,#5383)) ;
#1514 = EDGE_LOOP('',(#5384,#5385,#5386,#5387)) ;
#1515 = EDGE_LOOP('',(#5388,#5389,#5390)) ;
#1516 = EDGE_LOOP('',(#5391,#5392)) ;
#1517 = EDGE_LOOP('',(#5393,#5394,#5395,#5396)) ;
#1518 = EDGE_LOOP('',(#5397,#5398)) ;
#1519 = EDGE_LOOP('',(#5399,#5400,#5401,#5402,#5403,#5404,#5405,#5406)) ;
#1520 = EDGE_LOOP('',(#5407,#5408,#5409,#5410,#5411,#5412,#5413,#5414)) ;
#1521 = EDGE_LOOP('',(#5415,#5416,#5417,#5418,#5419,#5420,#5421,#5422)) ;
#1522 = EDGE_LOOP('',(#5423,#5424,#5425,#5426,#5427,#5428,#5429,#5430)) ;
#1523 = EDGE_LOOP('',(#5431,#5432,#5433,#5434)) ;
#1524 = EDGE_LOOP('',(#5435,#5436,#5437,#5438)) ;
#1525 = EDGE_LOOP('',(#5439,#5440,#5441,#5442)) ;
#1526 = EDGE_LOOP('',(#5443,#5444,#5445,#5446)) ;
#1527 = EDGE_LOOP('',(#5447,#5448,#5449,#5450)) ;
#1528 = EDGE_LOOP('',(#5451,#5452,#5453,#5454)) ;
#1529 = EDGE_LOOP('',(#5455,#5456,#5457,#5458)) ;
#1530 = EDGE_LOOP('',(#5459,#5460,#5461,#5462)) ;
#1531 = EDGE_LOOP('',(#5463,#5464,#5465,#5466)) ;
#1532 = EDGE_LOOP('',(#5467,#5468,#5469,#5470)) ;
#1533 = EDGE_LOOP('',(#5471,#5472,#5473,#5474)) ;
#1534 = EDGE_LOOP('',(#5475,#5476,#5477,#5478)) ;
#1535 = EDGE_LOOP('',(#5479,#5480,#5481,#5482,#5483,#5484,#5485,#5486)) ;
#1536 = EDGE_LOOP('',(#5487)) ;
#1537 = EDGE_LOOP('',(#5488,#5489,#5490,#5491)) ;
#1538 = EDGE_LOOP('',(#5492,#5493,#5494,#5495)) ;
#1539 = EDGE_LOOP('',(#5496,#5497,#5498,#5499,#5500,#5501,#5502,#5503)) ;
#1540 = EDGE_LOOP('',(#5504)) ;
#1541 = EDGE_LOOP('',(#5505,#5506,#5507,#5508,#5509,#5510,#5511,#5512,#5513,
#5514,#5515,#5516)) ;
#1542 = EDGE_LOOP('',(#5517,#5518,#5519,#5520)) ;
#1543 = EDGE_LOOP('',(#5521,#5522,#5523,#5524)) ;
#1544 = EDGE_LOOP('',(#5525,#5526,#5527,#5528)) ;
#1545 = EDGE_LOOP('',(#5529,#5530,#5531,#5532)) ;
#1546 = EDGE_LOOP('',(#5533,#5534,#5535,#5536)) ;
#1547 = EDGE_LOOP('',(#5537,#5538,#5539,#5540)) ;
#1548 = EDGE_LOOP('',(#5541,#5542,#5543,#5544)) ;
#1549 = EDGE_LOOP('',(#5545,#5546,#5547,#5548)) ;
#1550 = EDGE_LOOP('',(#5549,#5550,#5551,#5552)) ;
#1551 = EDGE_LOOP('',(#5553,#5554,#5555,#5556)) ;
#1552 = EDGE_LOOP('',(#5557,#5558,#5559,#5560)) ;
#1553 = EDGE_LOOP('',(#5561,#5562,#5563,#5564)) ;
#1554 = EDGE_LOOP('',(#5565,#5566,#5567,#5568)) ;
#1555 = EDGE_LOOP('',(#5569,#5570,#5571,#5572)) ;
#1556 = EDGE_LOOP('',(#5573,#5574,#5575,#5576)) ;
#1557 = EDGE_LOOP('',(#5577,#5578,#5579,#5580)) ;
#1558 = EDGE_LOOP('',(#5581,#5582,#5583,#5584)) ;
#1559 = EDGE_LOOP('',(#5585,#5586,#5587,#5588)) ;
#1560 = EDGE_LOOP('',(#5589,#5590,#5591,#5592)) ;
#1561 = EDGE_LOOP('',(#5593,#5594,#5595,#5596)) ;
#1562 = EDGE_LOOP('',(#5597,#5598,#5599,#5600)) ;
#1563 = EDGE_LOOP('',(#5601,#5602,#5603,#5604)) ;
#1564 = EDGE_LOOP('',(#5605,#5606,#5607,#5608)) ;
#1565 = EDGE_LOOP('',(#5609,#5610,#5611,#5612)) ;
#1566 = EDGE_LOOP('',(#5613,#5614,#5615,#5616)) ;
#1567 = EDGE_LOOP('',(#5617,#5618,#5619,#5620)) ;
#1568 = EDGE_LOOP('',(#5621,#5622,#5623,#5624)) ;
#1569 = EDGE_LOOP('',(#5625,#5626,#5627,#5628)) ;
#1570 = EDGE_LOOP('',(#5629,#5630,#5631,#5632)) ;
#1571 = EDGE_LOOP('',(#5633,#5634,#5635,#5636)) ;
#1572 = EDGE_LOOP('',(#5637,#5638,#5639,#5640,#5641,#5642,#5643,#5644,#5645,
#5646,#5647,#5648,#5649,#5650,#5651,#5652,#5653,#5654,#5655)) ;
#1573 = EDGE_LOOP('',(#5656,#5657,#5658,#5659,#5660,#5661,#5662,#5663,#5664)) ;
#1574 = EDGE_LOOP('',(#5665,#5666,#5667,#5668)) ;
#1575 = EDGE_LOOP('',(#5669,#5670,#5671,#5672)) ;
#1576 = EDGE_LOOP('',(#5673,#5674,#5675,#5676)) ;
#1577 = EDGE_LOOP('',(#5677,#5678,#5679,#5680)) ;
#1578 = EDGE_LOOP('',(#5681,#5682,#5683,#5684)) ;
#1579 = EDGE_LOOP('',(#5685,#5686,#5687,#5688)) ;
#1580 = EDGE_LOOP('',(#5689,#5690,#5691,#5692)) ;
#1581 = EDGE_LOOP('',(#5693,#5694,#5695,#5696)) ;
#1582 = EDGE_LOOP('',(#5697,#5698,#5699,#5700)) ;
#1583 = EDGE_LOOP('',(#5701,#5702,#5703,#5704,#5705,#5706,#5707,#5708,#5709)) ;
#1584 = EDGE_LOOP('',(#5710,#5711,#5712,#5713)) ;
#1585 = EDGE_LOOP('',(#5714,#5715,#5716,#5717,#5718,#5719,#5720,#5721,#5722,
#5723,#5724,#5725,#5726,#5727,#5728)) ;
#1586 = EDGE_LOOP('',(#5729,#5730,#5731,#5732,#5733,#5734,#5735,#5736,#5737,
#5738,#5739,#5740,#5741,#5742,#5743,#5744,#5745,#5746,#5747,#5748,#5749,
#5750,#5751,#5752,#5753,#5754,#5755,#5756,#5757,#5758,#5759,#5760,#5761,
#5762,#5763)) ;
#1587 = EDGE_LOOP('',(#5764,#5765,#5766,#5767,#5768,#5769,#5770,#5771,#5772,
#5773,#5774,#5775,#5776,#5777,#5778,#5779,#5780)) ;
#1588 = EDGE_LOOP('',(#5781,#5782,#5783,#5784,#5785,#5786,#5787,#5788,#5789,
#5790,#5791,#5792,#5793,#5794,#5795)) ;
#1589 = EDGE_LOOP('',(#5796,#5797,#5798,#5799)) ;
#1590 = EDGE_LOOP('',(#5800,#5801,#5802,#5803)) ;
#1591 = EDGE_LOOP('',(#5804,#5805,#5806,#5807,#5808,#5809,#5810,#5811,#5812)) ;
#1592 = EDGE_LOOP('',(#5813,#5814,#5815,#5816,#5817,#5818,#5819,#5820,#5821,
#5822,#5823,#5824,#5825,#5826,#5827,#5828,#5829,#5830,#5831)) ;
#1593 = EDGE_LOOP('',(#5832,#5833,#5834,#5835)) ;
#1594 = EDGE_LOOP('',(#5836,#5837,#5838,#5839)) ;
#1595 = EDGE_LOOP('',(#5840,#5841,#5842,#5843)) ;
#1596 = EDGE_LOOP('',(#5844,#5845,#5846,#5847)) ;
#1597 = EDGE_LOOP('',(#5848,#5849,#5850,#5851)) ;
#1598 = EDGE_LOOP('',(#5852,#5853,#5854,#5855)) ;
#1599 = EDGE_LOOP('',(#5856,#5857,#5858,#5859)) ;
#1600 = EDGE_LOOP('',(#5860,#5861,#5862,#5863)) ;
#1601 = EDGE_LOOP('',(#5864,#5865,#5866,#5867)) ;
#1602 = EDGE_LOOP('',(#5868,#5869,#5870,#5871)) ;
#1603 = EDGE_LOOP('',(#5872,#5873,#5874,#5875)) ;
#1604 = EDGE_LOOP('',(#5876,#5877,#5878,#5879)) ;
#1605 = EDGE_LOOP('',(#5880,#5881,#5882,#5883)) ;
#1606 = EDGE_LOOP('',(#5884,#5885,#5886,#5887)) ;
#1607 = EDGE_LOOP('',(#5888,#5889,#5890,#5891)) ;
#1608 = EDGE_LOOP('',(#5892,#5893,#5894,#5895)) ;
#1609 = EDGE_LOOP('',(#5896,#5897,#5898,#5899)) ;
#1610 = EDGE_LOOP('',(#5900,#5901,#5902,#5903)) ;
#1611 = EDGE_LOOP('',(#5904,#5905,#5906,#5907)) ;
#1612 = EDGE_LOOP('',(#5908,#5909,#5910,#5911)) ;
#1613 = EDGE_LOOP('',(#5912,#5913,#5914,#5915)) ;
#1614 = EDGE_LOOP('',(#5916,#5917,#5918,#5919)) ;
#1615 = EDGE_LOOP('',(#5920,#5921,#5922,#5923)) ;
#1616 = EDGE_LOOP('',(#5924,#5925,#5926,#5927)) ;
#1617 = EDGE_LOOP('',(#5928,#5929,#5930,#5931)) ;
#1618 = EDGE_LOOP('',(#5932,#5933,#5934,#5935,#5936,#5937,#5938,#5939,#5940,
#5941,#5942,#5943,#5944,#5945,#5946)) ;
#1619 = EDGE_LOOP('',(#5947,#5948,#5949,#5950)) ;
#1620 = EDGE_LOOP('',(#5951,#5952,#5953,#5954)) ;
#1621 = EDGE_LOOP('',(#5955,#5956,#5957,#5958)) ;
#1622 = EDGE_LOOP('',(#5959,#5960,#5961,#5962)) ;
#1623 = EDGE_LOOP('',(#5963,#5964,#5965,#5966)) ;
#1624 = EDGE_LOOP('',(#5967,#5968,#5969,#5970)) ;
#1625 = EDGE_LOOP('',(#5971,#5972,#5973,#5974)) ;
#1626 = EDGE_LOOP('',(#5975,#5976,#5977,#5978)) ;
#1627 = EDGE_LOOP('',(#5979,#5980,#5981,#5982)) ;
#1628 = EDGE_LOOP('',(#5983,#5984,#5985,#5986)) ;
#1629 = EDGE_LOOP('',(#5987,#5988,#5989,#5990)) ;
#1630 = EDGE_LOOP('',(#5991,#5992,#5993,#5994)) ;
#1631 = EDGE_LOOP('',(#5995,#5996,#5997,#5998)) ;
#1632 = EDGE_LOOP('',(#5999,#6000,#6001,#6002)) ;
#1633 = EDGE_LOOP('',(#6003,#6004,#6005,#6006)) ;
#1634 = EDGE_LOOP('',(#6007,#6008,#6009,#6010)) ;
#1635 = EDGE_LOOP('',(#6011,#6012,#6013,#6014)) ;
#1636 = EDGE_LOOP('',(#6015,#6016,#6017,#6018,#6019,#6020,#6021,#6022,#6023,
#6024,#6025,#6026,#6027,#6028,#6029,#6030,#6031)) ;
#1637 = EDGE_LOOP('',(#6032,#6033,#6034,#6035)) ;
#1638 = EDGE_LOOP('',(#6036,#6037,#6038,#6039)) ;
#1639 = EDGE_LOOP('',(#6040,#6041,#6042,#6043)) ;
#1640 = EDGE_LOOP('',(#6044,#6045,#6046,#6047)) ;
#1641 = EDGE_LOOP('',(#6048,#6049,#6050,#6051)) ;
#1642 = EDGE_LOOP('',(#6052,#6053,#6054,#6055)) ;
#1643 = EDGE_LOOP('',(#6056,#6057,#6058,#6059)) ;
#1644 = EDGE_LOOP('',(#6060,#6061,#6062,#6063)) ;
#1645 = EDGE_LOOP('',(#6064,#6065,#6066,#6067)) ;
#1646 = EDGE_LOOP('',(#6068,#6069,#6070,#6071)) ;
#1647 = EDGE_LOOP('',(#6072,#6073,#6074,#6075)) ;
#1648 = EDGE_LOOP('',(#6076,#6077,#6078,#6079)) ;
#1649 = EDGE_LOOP('',(#6080,#6081,#6082,#6083)) ;
#1650 = EDGE_LOOP('',(#6084,#6085,#6086,#6087)) ;
#1651 = EDGE_LOOP('',(#6088,#6089,#6090,#6091)) ;
#1652 = EDGE_LOOP('',(#6092,#6093,#6094,#6095)) ;
#1653 = EDGE_LOOP('',(#6096,#6097,#6098,#6099)) ;
#1654 = EDGE_LOOP('',(#6100,#6101,#6102,#6103)) ;
#1655 = EDGE_LOOP('',(#6104,#6105,#6106,#6107)) ;
#1656 = EDGE_LOOP('',(#6108,#6109,#6110,#6111)) ;
#1657 = EDGE_LOOP('',(#6112,#6113,#6114,#6115)) ;
#1658 = EDGE_LOOP('',(#6116,#6117,#6118,#6119)) ;
#1659 = EDGE_LOOP('',(#6120,#6121,#6122,#6123)) ;
#1660 = EDGE_LOOP('',(#6124,#6125,#6126,#6127)) ;
#1661 = EDGE_LOOP('',(#6128,#6129,#6130,#6131)) ;
#1662 = EDGE_LOOP('',(#6132,#6133,#6134,#6135)) ;
#1663 = EDGE_LOOP('',(#6136,#6137,#6138,#6139)) ;
#1664 = EDGE_LOOP('',(#6140,#6141,#6142,#6143)) ;
#1665 = EDGE_LOOP('',(#6144,#6145,#6146,#6147)) ;
#1666 = EDGE_LOOP('',(#6148,#6149,#6150,#6151)) ;
#1667 = EDGE_LOOP('',(#6152,#6153,#6154,#6155)) ;
#1668 = EDGE_LOOP('',(#6156,#6157,#6158,#6159)) ;
#1669 = EDGE_LOOP('',(#6160,#6161,#6162,#6163)) ;
#1670 = EDGE_LOOP('',(#6164,#6165,#6166,#6167)) ;
#1671 = EDGE_LOOP('',(#6168,#6169,#6170,#6171)) ;
#1672 = EDGE_LOOP('',(#6172,#6173,#6174,#6175,#6176,#6177,#6178,#6179,#6180,
#6181,#6182,#6183,#6184,#6185,#6186,#6187,#6188,#6189,#6190,#6191,#6192,
#6193,#6194,#6195,#6196,#6197,#6198,#6199,#6200,#6201,#6202,#6203,#6204,
#6205,#6206)) ;
#1673 = EDGE_LOOP('',(#6207,#6208,#6209,#6210)) ;
#1674 = EDGE_LOOP('',(#6211,#6212,#6213,#6214)) ;
#1675 = EDGE_LOOP('',(#6215,#6216,#6217,#6218)) ;
#1676 = EDGE_LOOP('',(#6219,#6220,#6221,#6222)) ;
#1677 = EDGE_LOOP('',(#6223,#6224,#6225,#6226)) ;
#1678 = EDGE_LOOP('',(#6227,#6228,#6229,#6230)) ;
#1679 = EDGE_LOOP('',(#6231,#6232,#6233,#6234)) ;
#1680 = EDGE_LOOP('',(#6235,#6236,#6237,#6238)) ;
#1681 = EDGE_LOOP('',(#6239,#6240,#6241,#6242)) ;
#1682 = EDGE_LOOP('',(#6243,#6244,#6245,#6246)) ;
#1683 = EDGE_LOOP('',(#6247,#6248,#6249,#6250)) ;
#1684 = EDGE_LOOP('',(#6251,#6252,#6253,#6254)) ;
#1685 = EDGE_LOOP('',(#6255,#6256,#6257,#6258)) ;
#1686 = EDGE_LOOP('',(#6259,#6260,#6261,#6262)) ;
#1687 = EDGE_LOOP('',(#6263,#6264,#6265,#6266)) ;
#1688 = EDGE_LOOP('',(#6267,#6268,#6269,#6270,#6271,#6272,#6273,#6274,#6275,
#6276,#6277,#6278,#6279,#6280,#6281)) ;
#1689 = EDGE_LOOP('',(#6282,#6283,#6284,#6285)) ;
#1690 = EDGE_LOOP('',(#6286)) ;
#1691 = EDGE_LOOP('',(#6287)) ;
#1692 = EDGE_LOOP('',(#6288)) ;
#1693 = EDGE_LOOP('',(#6289)) ;
#1694 = EDGE_LOOP('',(#6290,#6291,#6292,#6293,#6294,#6295,#6296,#6297,#6298)) ;
#1695 = EDGE_LOOP('',(#6299,#6300,#6301,#6302,#6303)) ;
#1696 = EDGE_LOOP('',(#6304,#6305,#6306,#6307)) ;
#1697 = EDGE_LOOP('',(#6308,#6309,#6310,#6311,#6312,#6313,#6314,#6315,#6316,
#6317,#6318,#6319,#6320)) ;
#1698 = EDGE_LOOP('',(#6321,#6322,#6323,#6324,#6325,#6326)) ;
#1699 = EDGE_LOOP('',(#6327,#6328,#6329,#6330,#6331)) ;
#1700 = EDGE_LOOP('',(#6332,#6333,#6334,#6335)) ;
#1701 = EDGE_LOOP('',(#6336,#6337,#6338,#6339,#6340,#6341)) ;
#1702 = EDGE_LOOP('',(#6342,#6343,#6344,#6345,#6346)) ;
#1703 = EDGE_LOOP('',(#6347,#6348,#6349,#6350)) ;
#1704 = EDGE_LOOP('',(#6351,#6352,#6353,#6354,#6355,#6356)) ;
#1705 = EDGE_LOOP('',(#6357,#6358,#6359,#6360,#6361)) ;
#1706 = EDGE_LOOP('',(#6362,#6363,#6364,#6365)) ;
#1707 = EDGE_LOOP('',(#6366,#6367,#6368,#6369,#6370,#6371)) ;
#1708 = EDGE_LOOP('',(#6372)) ;
#1709 = EDGE_LOOP('',(#6373)) ;
#1710 = EDGE_LOOP('',(#6374)) ;
#1711 = EDGE_LOOP('',(#6375)) ;
#1712 = EDGE_LOOP('',(#6376)) ;
#1713 = EDGE_LOOP('',(#6377)) ;
#1714 = EDGE_LOOP('',(#6378)) ;
#1715 = EDGE_LOOP('',(#6379)) ;
#1716 = EDGE_LOOP('',(#6380,#6381,#6382,#6383)) ;
#1717 = EDGE_LOOP('',(#6384,#6385,#6386,#6387)) ;
#1718 = EDGE_LOOP('',(#6388,#6389,#6390,#6391)) ;
#1719 = EDGE_LOOP('',(#6392,#6393,#6394,#6395)) ;
#1720 = EDGE_LOOP('',(#6396,#6397,#6398,#6399)) ;
#1721 = EDGE_LOOP('',(#6400,#6401,#6402,#6403)) ;
#1722 = EDGE_LOOP('',(#6404,#6405,#6406,#6407)) ;
#1723 = EDGE_LOOP('',(#6408,#6409,#6410,#6411)) ;
#1724 = EDGE_LOOP('',(#6412)) ;
#1725 = EDGE_LOOP('',(#6413,#6414,#6415,#6416,#6417,#6418,#6419,#6420)) ;
#1726 = EDGE_LOOP('',(#6421,#6422,#6423,#6424)) ;
#1727 = EDGE_LOOP('',(#6425,#6426,#6427,#6428)) ;
#1728 = EDGE_LOOP('',(#6429,#6430,#6431,#6432)) ;
#1729 = EDGE_LOOP('',(#6433,#6434,#6435,#6436)) ;
#1730 = EDGE_LOOP('',(#6437)) ;
#1731 = EDGE_LOOP('',(#6438,#6439,#6440,#6441,#6442,#6443,#6444,#6445,#6446)) ;
#1732 = EDGE_LOOP('',(#6447,#6448,#6449,#6450,#6451)) ;
#1733 = EDGE_LOOP('',(#6452)) ;
#1734 = EDGE_LOOP('',(#6453)) ;
#1735 = EDGE_LOOP('',(#6454,#6455,#6456,#6457)) ;
#1736 = EDGE_LOOP('',(#6458)) ;
#1737 = EDGE_LOOP('',(#6459)) ;
#1738 = EDGE_LOOP('',(#6460,#6461,#6462,#6463)) ;
#1739 = EDGE_LOOP('',(#6464)) ;
#1740 = EDGE_LOOP('',(#6465)) ;
#1741 = EDGE_LOOP('',(#6466,#6467,#6468,#6469)) ;
#1742 = EDGE_LOOP('',(#6470)) ;
#1743 = EDGE_LOOP('',(#6471)) ;
#1744 = EDGE_LOOP('',(#6472,#6473,#6474,#6475)) ;
#1745 = EDGE_LOOP('',(#6476)) ;
#1746 = EDGE_LOOP('',(#6477,#6478,#6479,#6480,#6481,#6482,#6483,#6484)) ;
#1747 = EDGE_LOOP('',(#6485,#6486,#6487,#6488)) ;
#1748 = EDGE_LOOP('',(#6489)) ;
#1749 = EDGE_LOOP('',(#6490)) ;
#1750 = EDGE_LOOP('',(#6491)) ;
#1751 = EDGE_LOOP('',(#6492)) ;
#1752 = EDGE_LOOP('',(#6493)) ;
#1753 = EDGE_LOOP('',(#6494)) ;
#1754 = EDGE_LOOP('',(#6495,#6496,#6497,#6498)) ;
#1755 = EDGE_LOOP('',(#6499,#6500,#6501,#6502)) ;
#1756 = EDGE_LOOP('',(#6503,#6504,#6505,#6506)) ;
#1757 = EDGE_LOOP('',(#6507,#6508,#6509,#6510)) ;
#1758 = EDGE_LOOP('',(#6511)) ;
#1759 = EDGE_LOOP('',(#6512)) ;
#1760 = EDGE_LOOP('',(#6513,#6514,#6515,#6516)) ;
#1761 = EDGE_LOOP('',(#6517,#6518,#6519,#6520)) ;
#1762 = EDGE_LOOP('',(#6521,#6522,#6523,#6524)) ;
#1763 = EDGE_LOOP('',(#6525,#6526,#6527,#6528)) ;
#1764 = EDGE_LOOP('',(#6529,#6530,#6531,#6532)) ;
#1765 = EDGE_LOOP('',(#6533,#6534,#6535,#6536)) ;
#1766 = EDGE_LOOP('',(#6537,#6538,#6539,#6540)) ;
#1767 = EDGE_LOOP('',(#6541,#6542,#6543,#6544)) ;
#1768 = EDGE_LOOP('',(#6545,#6546,#6547,#6548)) ;
#1769 = EDGE_LOOP('',(#6549,#6550,#6551,#6552)) ;
#1770 = EDGE_LOOP('',(#6553,#6554,#6555,#6556)) ;
#1771 = EDGE_LOOP('',(#6557,#6558,#6559,#6560)) ;
#1772 = EDGE_LOOP('',(#6561,#6562,#6563,#6564)) ;
#1773 = EDGE_LOOP('',(#6565,#6566,#6567,#6568)) ;
#1774 = EDGE_LOOP('',(#6569,#6570,#6571,#6572)) ;
#1775 = EDGE_LOOP('',(#6573,#6574,#6575,#6576)) ;
#1776 = EDGE_LOOP('',(#6577,#6578,#6579,#6580)) ;
#1777 = EDGE_LOOP('',(#6581,#6582,#6583,#6584)) ;
#1778 = EDGE_LOOP('',(#6585,#6586,#6587,#6588)) ;
#1779 = EDGE_LOOP('',(#6589,#6590,#6591,#6592)) ;
#1780 = EDGE_LOOP('',(#6593,#6594,#6595,#6596)) ;
#1781 = EDGE_LOOP('',(#6597,#6598,#6599,#6600)) ;
#1782 = EDGE_LOOP('',(#6601)) ;
#1783 = EDGE_LOOP('',(#6602)) ;
#1784 = EDGE_LOOP('',(#6603,#6604,#6605,#6606)) ;
#1785 = EDGE_LOOP('',(#6607,#6608,#6609,#6610)) ;
#1786 = EDGE_LOOP('',(#6611,#6612,#6613,#6614)) ;
#1787 = EDGE_LOOP('',(#6615,#6616,#6617,#6618)) ;
#1788 = EDGE_LOOP('',(#6619,#6620,#6621,#6622)) ;
#1789 = EDGE_LOOP('',(#6623)) ;
#1790 = EDGE_LOOP('',(#6624)) ;
#1791 = EDGE_LOOP('',(#6625,#6626)) ;
#1792 = EDGE_LOOP('',(#6627,#6628,#6629,#6630)) ;
#1793 = EDGE_LOOP('',(#6631,#6632,#6633,#6634)) ;
#1794 = EDGE_LOOP('',(#6635,#6636,#6637,#6638)) ;
#1795 = EDGE_LOOP('',(#6639,#6640,#6641,#6642)) ;
#1796 = EDGE_LOOP('',(#6643,#6644,#6645,#6646)) ;
#1797 = EDGE_LOOP('',(#6647,#6648,#6649,#6650)) ;
#1798 = EDGE_LOOP('',(#6651,#6652,#6653,#6654)) ;
#1799 = EDGE_LOOP('',(#6655,#6656,#6657,#6658)) ;
#1800 = EDGE_LOOP('',(#6659,#6660,#6661,#6662)) ;
#1801 = EDGE_LOOP('',(#6663,#6664,#6665,#6666)) ;
#1802 = EDGE_LOOP('',(#6667,#6668,#6669,#6670)) ;
#1803 = EDGE_LOOP('',(#6671,#6672,#6673,#6674)) ;
#1804 = EDGE_LOOP('',(#6675,#6676,#6677,#6678)) ;
#1805 = EDGE_LOOP('',(#6679,#6680,#6681,#6682,#6683)) ;
#1806 = EDGE_LOOP('',(#6684,#6685,#6686,#6687)) ;
#1807 = EDGE_LOOP('',(#6688,#6689,#6690,#6691)) ;
#1808 = EDGE_LOOP('',(#6692,#6693,#6694,#6695)) ;
#1809 = EDGE_LOOP('',(#6696,#6697,#6698,#6699)) ;
#1810 = EDGE_LOOP('',(#6700,#6701,#6702,#6703)) ;
#1811 = EDGE_LOOP('',(#6704,#6705,#6706,#6707)) ;
#1812 = EDGE_LOOP('',(#6708,#6709,#6710,#6711)) ;
#1813 = EDGE_LOOP('',(#6712,#6713,#6714,#6715)) ;
#1814 = EDGE_LOOP('',(#6716,#6717,#6718,#6719)) ;
#1815 = EDGE_LOOP('',(#6720,#6721,#6722,#6723)) ;
#1816 = EDGE_LOOP('',(#6724,#6725,#6726,#6727)) ;
#1817 = EDGE_LOOP('',(#6728,#6729,#6730,#6731)) ;
#1818 = EDGE_LOOP('',(#6732,#6733,#6734,#6735)) ;
#1819 = EDGE_LOOP('',(#6736,#6737,#6738,#6739)) ;
#1820 = EDGE_LOOP('',(#6740,#6741,#6742,#6743,#6744,#6745,#6746,#6747,#6748,
#6749,#6750,#6751,#6752,#6753,#6754,#6755,#6756,#6757,#6758,#6759,#6760,
#6761,#6762,#6763,#6764,#6765,#6766,#6767,#6768,#6769,#6770)) ;
#1821 = EDGE_LOOP('',(#6771,#6772,#6773,#6774,#6775)) ;
#1822 = EDGE_LOOP('',(#6776,#6777,#6778,#6779)) ;
#1823 = EDGE_LOOP('',(#6780,#6781,#6782,#6783,#6784,#6785,#6786,#6787,#6788,
#6789,#6790,#6791,#6792,#6793,#6794,#6795,#6796,#6797,#6798,#6799,#6800,
#6801,#6802,#6803,#6804,#6805,#6806,#6807,#6808,#6809)) ;
#1824 = EDGE_LOOP('',(#6810,#6811,#6812,#6813,#6814,#6815)) ;
#1825 = EDGE_LOOP('',(#6816,#6817,#6818)) ;
#1826 = EDGE_LOOP('',(#6819)) ;
#1827 = EDGE_LOOP('',(#6820)) ;
#1828 = EDGE_LOOP('',(#6821,#6822,#6823,#6824,#6825,#6826)) ;
#1829 = EDGE_LOOP('',(#6827)) ;
#1830 = EDGE_LOOP('',(#6828,#6829,#6830,#6831)) ;
#1831 = EDGE_LOOP('',(#6832,#6833,#6834)) ;
#1832 = EDGE_LOOP('',(#6835,#6836,#6837,#6838)) ;
#1833 = EDGE_LOOP('',(#6839,#6840,#6841,#6842,#6843,#6844,#6845,#6846,#6847,
#6848,#6849,#6850,#6851,#6852,#6853,#6854,#6855,#6856,#6857,#6858,#6859,
#6860,#6861,#6862,#6863,#6864,#6865,#6866,#6867,#6868,#6869,#6870,#6871,
#6872,#6873,#6874,#6875,#6876,#6877,#6878,#6879,#6880,#6881,#6882,#6883,
#6884,#6885,#6886,#6887,#6888,#6889,#6890,#6891,#6892,#6893,#6894,#6895,
#6896,#6897,#6898,#6899,#6900,#6901,#6902,#6903,#6904,#6905,#6906,#6907,
#6908,#6909,#6910,#6911,#6912,#6913,#6914,#6915,#6916,#6917,#6918,#6919,
#6920,#6921,#6922,#6923,#6924,#6925,#6926,#6927,#6928,#6929,#6930,#6931,
#6932,#6933,#6934,#6935,#6936,#6937,#6938,#6939,#6940,#6941,#6942,#6943,
#6944,#6945,#6946,#6947,#6948,#6949,#6950,#6951,#6952,#6953,#6954,#6955,
#6956,#6957,#6958,#6959,#6960,#6961,#6962,#6963,#6964,#6965,#6966,#6967,
#6968,#6969,#6970,#6971,#6972,#6973,#6974,#6975,#6976,#6977,#6978,#6979,
#6980,#6981,#6982,#6983,#6984,#6985,#6986)) ;
#1834 = EDGE_LOOP('',(#6987,#6988,#6989,#6990)) ;
#1835 = EDGE_LOOP('',(#6991,#6992,#6993)) ;
#1836 = EDGE_LOOP('',(#6994,#6995,#6996,#6997)) ;
#1837 = EDGE_LOOP('',(#6998,#6999,#7000,#7001)) ;
#1838 = EDGE_LOOP('',(#7002,#7003,#7004)) ;
#1839 = EDGE_LOOP('',(#7005,#7006,#7007,#7008)) ;
#1840 = EDGE_LOOP('',(#7009,#7010,#7011,#7012)) ;
#1841 = EDGE_LOOP('',(#7013,#7014,#7015)) ;
#1842 = EDGE_LOOP('',(#7016,#7017,#7018,#7019)) ;
#1843 = EDGE_LOOP('',(#7020,#7021,#7022,#7023)) ;
#1844 = EDGE_LOOP('',(#7024,#7025,#7026)) ;
#1845 = EDGE_LOOP('',(#7027,#7028,#7029,#7030)) ;
#1846 = EDGE_LOOP('',(#7031,#7032,#7033,#7034)) ;
#1847 = EDGE_LOOP('',(#7035,#7036,#7037)) ;
#1848 = EDGE_LOOP('',(#7038,#7039,#7040,#7041)) ;
#1849 = EDGE_LOOP('',(#7042,#7043,#7044,#7045)) ;
#1850 = EDGE_LOOP('',(#7046,#7047,#7048)) ;
#1851 = EDGE_LOOP('',(#7049,#7050,#7051,#7052)) ;
#1852 = EDGE_LOOP('',(#7053,#7054,#7055,#7056)) ;
#1853 = EDGE_LOOP('',(#7057,#7058,#7059)) ;
#1854 = EDGE_LOOP('',(#7060,#7061,#7062,#7063)) ;
#1855 = EDGE_LOOP('',(#7064,#7065,#7066,#7067)) ;
#1856 = EDGE_LOOP('',(#7068,#7069,#7070,#7071)) ;
#1857 = EDGE_LOOP('',(#7072,#7073,#7074,#7075)) ;
#1858 = EDGE_LOOP('',(#7076,#7077,#7078,#7079)) ;
#1859 = EDGE_LOOP('',(#7080,#7081,#7082)) ;
#1860 = EDGE_LOOP('',(#7083,#7084,#7085,#7086)) ;
#1861 = EDGE_LOOP('',(#7087,#7088,#7089,#7090)) ;
#1862 = EDGE_LOOP('',(#7091,#7092,#7093)) ;
#1863 = EDGE_LOOP('',(#7094,#7095,#7096,#7097)) ;
#1864 = EDGE_LOOP('',(#7098,#7099,#7100,#7101)) ;
#1865 = EDGE_LOOP('',(#7102,#7103,#7104)) ;
#1866 = EDGE_LOOP('',(#7105,#7106,#7107,#7108)) ;
#1867 = EDGE_LOOP('',(#7109,#7110,#7111,#7112)) ;
#1868 = EDGE_LOOP('',(#7113,#7114,#7115)) ;
#1869 = EDGE_LOOP('',(#7116,#7117,#7118,#7119)) ;
#1870 = EDGE_LOOP('',(#7120,#7121,#7122,#7123)) ;
#1871 = EDGE_LOOP('',(#7124,#7125,#7126)) ;
#1872 = EDGE_LOOP('',(#7127,#7128,#7129,#7130)) ;
#1873 = EDGE_LOOP('',(#7131,#7132,#7133,#7134)) ;
#1874 = EDGE_LOOP('',(#7135,#7136,#7137)) ;
#1875 = EDGE_LOOP('',(#7138,#7139,#7140,#7141)) ;
#1876 = EDGE_LOOP('',(#7142,#7143,#7144,#7145)) ;
#1877 = EDGE_LOOP('',(#7146,#7147,#7148)) ;
#1878 = EDGE_LOOP('',(#7149,#7150,#7151,#7152)) ;
#1879 = EDGE_LOOP('',(#7153,#7154,#7155,#7156)) ;
#1880 = EDGE_LOOP('',(#7157,#7158,#7159)) ;
#1881 = EDGE_LOOP('',(#7160,#7161,#7162,#7163)) ;
#1882 = EDGE_LOOP('',(#7164,#7165,#7166,#7167)) ;
#1883 = EDGE_LOOP('',(#7168,#7169,#7170)) ;
#1884 = EDGE_LOOP('',(#7171,#7172,#7173,#7174)) ;
#1885 = EDGE_LOOP('',(#7175,#7176,#7177,#7178)) ;
#1886 = EDGE_LOOP('',(#7179,#7180,#7181)) ;
#1887 = EDGE_LOOP('',(#7182,#7183,#7184,#7185)) ;
#1888 = EDGE_LOOP('',(#7186,#7187,#7188,#7189)) ;
#1889 = EDGE_LOOP('',(#7190,#7191,#7192)) ;
#1890 = EDGE_LOOP('',(#7193,#7194,#7195,#7196)) ;
#1891 = EDGE_LOOP('',(#7197,#7198,#7199,#7200)) ;
#1892 = EDGE_LOOP('',(#7201,#7202,#7203)) ;
#1893 = EDGE_LOOP('',(#7204,#7205,#7206,#7207)) ;
#1894 = EDGE_LOOP('',(#7208,#7209,#7210,#7211)) ;
#1895 = EDGE_LOOP('',(#7212,#7213,#7214)) ;
#1896 = EDGE_LOOP('',(#7215,#7216,#7217,#7218)) ;
#1897 = EDGE_LOOP('',(#7219,#7220,#7221,#7222)) ;
#1898 = EDGE_LOOP('',(#7223,#7224,#7225)) ;
#1899 = EDGE_LOOP('',(#7226,#7227,#7228,#7229)) ;
#1900 = EDGE_LOOP('',(#7230,#7231,#7232,#7233)) ;
#1901 = EDGE_LOOP('',(#7234,#7235,#7236)) ;
#1902 = EDGE_LOOP('',(#7237,#7238,#7239,#7240)) ;
#1903 = EDGE_LOOP('',(#7241,#7242,#7243,#7244)) ;
#1904 = EDGE_LOOP('',(#7245,#7246,#7247)) ;
#1905 = EDGE_LOOP('',(#7248,#7249,#7250,#7251)) ;
#1906 = EDGE_LOOP('',(#7252,#7253,#7254,#7255)) ;
#1907 = EDGE_LOOP('',(#7256,#7257,#7258)) ;
#1908 = EDGE_LOOP('',(#7259,#7260,#7261,#7262)) ;
#1909 = EDGE_LOOP('',(#7263,#7264,#7265,#7266)) ;
#1910 = EDGE_LOOP('',(#7267,#7268,#7269)) ;
#1911 = EDGE_LOOP('',(#7270,#7271,#7272,#7273)) ;
#1912 = EDGE_LOOP('',(#7274,#7275,#7276,#7277)) ;
#1913 = EDGE_LOOP('',(#7278,#7279,#7280)) ;
#1914 = EDGE_LOOP('',(#7281,#7282,#7283,#7284)) ;
#1915 = EDGE_LOOP('',(#7285,#7286,#7287,#7288)) ;
#1916 = EDGE_LOOP('',(#7289,#7290,#7291)) ;
#1917 = EDGE_LOOP('',(#7292,#7293,#7294,#7295)) ;
#1918 = EDGE_LOOP('',(#7296,#7297,#7298,#7299)) ;
#1919 = EDGE_LOOP('',(#7300,#7301,#7302)) ;
#1920 = EDGE_LOOP('',(#7303,#7304,#7305,#7306)) ;
#1921 = EDGE_LOOP('',(#7307,#7308,#7309,#7310)) ;
#1922 = EDGE_LOOP('',(#7311,#7312,#7313)) ;
#1923 = EDGE_LOOP('',(#7314,#7315,#7316,#7317)) ;
#1924 = EDGE_LOOP('',(#7318,#7319,#7320,#7321)) ;
#1925 = EDGE_LOOP('',(#7322,#7323,#7324)) ;
#1926 = EDGE_LOOP('',(#7325,#7326,#7327,#7328)) ;
#1927 = EDGE_LOOP('',(#7329,#7330,#7331,#7332)) ;
#1928 = EDGE_LOOP('',(#7333,#7334,#7335)) ;
#1929 = EDGE_LOOP('',(#7336,#7337,#7338,#7339)) ;
#1930 = EDGE_LOOP('',(#7340,#7341,#7342,#7343)) ;
#1931 = EDGE_LOOP('',(#7344,#7345,#7346)) ;
#1932 = EDGE_LOOP('',(#7347,#7348,#7349,#7350)) ;
#1933 = EDGE_LOOP('',(#7351,#7352,#7353,#7354)) ;
#1934 = EDGE_LOOP('',(#7355,#7356,#7357)) ;
#1935 = EDGE_LOOP('',(#7358,#7359,#7360,#7361)) ;
#1936 = EDGE_LOOP('',(#7362,#7363,#7364,#7365)) ;
#1937 = EDGE_LOOP('',(#7366,#7367,#7368)) ;
#1938 = EDGE_LOOP('',(#7369,#7370,#7371,#7372)) ;
#1939 = EDGE_LOOP('',(#7373,#7374,#7375,#7376)) ;
#1940 = EDGE_LOOP('',(#7377,#7378,#7379,#7380,#7381,#7382,#7383,#7384,#7385,
#7386,#7387,#7388,#7389,#7390,#7391,#7392,#7393,#7394,#7395,#7396,#7397,
#7398,#7399,#7400,#7401,#7402,#7403,#7404,#7405,#7406,#7407,#7408,#7409,
#7410,#7411,#7412,#7413,#7414,#7415,#7416,#7417,#7418,#7419,#7420,#7421,
#7422,#7423,#7424,#7425,#7426,#7427,#7428,#7429,#7430,#7431,#7432,#7433,
#7434,#7435,#7436,#7437,#7438,#7439,#7440,#7441,#7442,#7443,#7444,#7445,
#7446,#7447,#7448,#7449,#7450,#7451,#7452,#7453,#7454,#7455,#7456,#7457,
#7458,#7459,#7460,#7461,#7462,#7463,#7464,#7465,#7466,#7467,#7468,#7469,
#7470,#7471,#7472,#7473,#7474,#7475,#7476,#7477,#7478,#7479,#7480,#7481,
#7482,#7483,#7484,#7485,#7486,#7487)) ;
#1941 = EDGE_LOOP('',(#7488)) ;
#1942 = EDGE_LOOP('',(#7489)) ;
#1943 = EDGE_LOOP('',(#7490,#7491,#7492,#7493,#7494,#7495,#7496,#7497,#7498,
#7499,#7500,#7501,#7502,#7503,#7504,#7505,#7506,#7507,#7508,#7509,#7510)) ;
#1944 = EDGE_LOOP('',(#7511,#7512,#7513,#7514)) ;
#1945 = EDGE_LOOP('',(#7515,#7516,#7517,#7518)) ;
#1946 = EDGE_LOOP('',(#7519,#7520,#7521,#7522)) ;
#1947 = EDGE_LOOP('',(#7523,#7524,#7525,#7526)) ;
#1948 = EDGE_LOOP('',(#7527,#7528,#7529,#7530)) ;
#1949 = EDGE_LOOP('',(#7531,#7532,#7533,#7534)) ;
#1950 = EDGE_LOOP('',(#7535,#7536,#7537,#7538,#7539,#7540,#7541,#7542)) ;
#1951 = EDGE_LOOP('',(#7543,#7544,#7545,#7546,#7547,#7548,#7549,#7550)) ;
#1952 = EDGE_LOOP('',(#7551,#7552,#7553,#7554,#7555,#7556,#7557,#7558)) ;
#1953 = EDGE_LOOP('',(#7559,#7560)) ;
#1954 = EDGE_LOOP('',(#7561,#7562)) ;
#1955 = EDGE_LOOP('',(#7563,#7564)) ;
#1956 = EDGE_LOOP('',(#7565,#7566)) ;
#1957 = EDGE_LOOP('',(#7567,#7568)) ;
#1958 = EDGE_LOOP('',(#7569,#7570)) ;
#1959 = EDGE_LOOP('',(#7571,#7572)) ;
#1960 = EDGE_LOOP('',(#7573,#7574)) ;
#1961 = EDGE_LOOP('',(#7575,#7576)) ;
#1962 = EDGE_LOOP('',(#7577,#7578)) ;
#1963 = EDGE_LOOP('',(#7579,#7580)) ;
#1964 = EDGE_LOOP('',(#7581,#7582)) ;
#1965 = EDGE_LOOP('',(#7583,#7584,#7585,#7586,#7587,#7588,#7589,#7590)) ;
#1966 = EDGE_LOOP('',(#7591,#7592,#7593,#7594,#7595,#7596,#7597,#7598)) ;
#1967 = EDGE_LOOP('',(#7599,#7600,#7601,#7602,#7603,#7604,#7605,#7606)) ;
#1968 = EDGE_LOOP('',(#7607,#7608,#7609,#7610,#7611,#7612,#7613,#7614)) ;
#1969 = EDGE_LOOP('',(#7615)) ;
#1970 = EDGE_LOOP('',(#7616)) ;
#1971 = EDGE_LOOP('',(#7617,#7618,#7619,#7620)) ;
#1972 = EDGE_LOOP('',(#7621)) ;
#1973 = EDGE_LOOP('',(#7622)) ;
#1974 = EDGE_LOOP('',(#7623,#7624,#7625,#7626)) ;
#1975 = EDGE_LOOP('',(#7627,#7628,#7629,#7630)) ;
#1976 = EDGE_LOOP('',(#7631,#7632,#7633,#7634)) ;
#1977 = EDGE_LOOP('',(#7635,#7636,#7637,#7638)) ;
#1978 = EDGE_LOOP('',(#7639,#7640,#7641,#7642)) ;
#1979 = EDGE_LOOP('',(#7643,#7644,#7645,#7646)) ;
#1980 = EDGE_LOOP('',(#7647,#7648,#7649,#7650)) ;
#1981 = EDGE_LOOP('',(#7651,#7652,#7653,#7654)) ;
#1982 = EDGE_LOOP('',(#7655,#7656,#7657,#7658)) ;
#1983 = EDGE_LOOP('',(#7659,#7660,#7661,#7662)) ;
#1984 = EDGE_LOOP('',(#7663,#7664,#7665,#7666,#7667,#7668,#7669,#7670)) ;
#1985 = EDGE_LOOP('',(#7671)) ;
#1986 = EDGE_LOOP('',(#7672)) ;
#1987 = EDGE_LOOP('',(#7673,#7674,#7675,#7676)) ;
#1988 = EDGE_LOOP('',(#7677,#7678,#7679,#7680)) ;
#1989 = EDGE_LOOP('',(#7681,#7682,#7683,#7684)) ;
#1990 = EDGE_LOOP('',(#7685,#7686,#7687,#7688)) ;
#1991 = EDGE_LOOP('',(#7689,#7690,#7691,#7692)) ;
#1992 = EDGE_LOOP('',(#7693,#7694,#7695,#7696)) ;
#1993 = EDGE_LOOP('',(#7697,#7698,#7699,#7700,#7701,#7702,#7703,#7704)) ;
#1994 = EDGE_LOOP('',(#7705)) ;
#1995 = EDGE_LOOP('',(#7706)) ;
#1996 = LINE('',#10958,#2558) ;
#1997 = LINE('',#10962,#2559) ;
#1998 = LINE('',#10971,#2560) ;
#1999 = LINE('',#10976,#2561) ;
#2000 = LINE('',#10980,#2562) ;
#2001 = LINE('',#10989,#2563) ;
#2002 = LINE('',#10995,#2564) ;
#2003 = LINE('',#10999,#2565) ;
#2004 = LINE('',#11001,#2566) ;
#2005 = LINE('',#11002,#2567) ;
#2006 = LINE('',#11011,#2568) ;
#2007 = LINE('',#11014,#2569) ;
#2008 = LINE('',#11016,#2570) ;
#2009 = LINE('',#11017,#2571) ;
#2010 = LINE('',#11040,#2572) ;
#2011 = LINE('',#11058,#2573) ;
#2012 = LINE('',#11079,#2574) ;
#2013 = LINE('',#11097,#2575) ;
#2014 = LINE('',#11109,#2576) ;
#2015 = LINE('',#11128,#2577) ;
#2016 = LINE('',#11148,#2578) ;
#2017 = LINE('',#11167,#2579) ;
#2018 = LINE('',#11210,#2580) ;
#2019 = LINE('',#11212,#2581) ;
#2020 = LINE('',#11219,#2582) ;
#2021 = LINE('',#11220,#2583) ;
#2022 = LINE('',#11222,#2584) ;
#2023 = LINE('',#11243,#2585) ;
#2024 = LINE('',#11248,#2586) ;
#2025 = LINE('',#11270,#2587) ;
#2026 = LINE('',#11292,#2588) ;
#2027 = LINE('',#11314,#2589) ;
#2028 = LINE('',#11334,#2590) ;
#2029 = LINE('',#11339,#2591) ;
#2030 = LINE('',#11358,#2592) ;
#2031 = LINE('',#11377,#2593) ;
#2032 = LINE('',#11396,#2594) ;
#2033 = LINE('',#11415,#2595) ;
#2034 = LINE('',#11437,#2596) ;
#2035 = LINE('',#11455,#2597) ;
#2036 = LINE('',#11475,#2598) ;
#2037 = LINE('',#11497,#2599) ;
#2038 = LINE('',#11516,#2600) ;
#2039 = LINE('',#11532,#2601) ;
#2040 = LINE('',#11551,#2602) ;
#2041 = LINE('',#11570,#2603) ;
#2042 = LINE('',#11608,#2604) ;
#2043 = LINE('',#11624,#2605) ;
#2044 = LINE('',#11643,#2606) ;
#2045 = LINE('',#11668,#2607) ;
#2046 = LINE('',#11687,#2608) ;
#2047 = LINE('',#11706,#2609) ;
#2048 = LINE('',#11728,#2610) ;
#2049 = LINE('',#11753,#2611) ;
#2050 = LINE('',#11761,#2612) ;
#2051 = LINE('',#11762,#2613) ;
#2052 = LINE('',#11796,#2614) ;
#2053 = LINE('',#11801,#2615) ;
#2054 = LINE('',#11806,#2616) ;
#2055 = LINE('',#11807,#2617) ;
#2056 = LINE('',#11826,#2618) ;
#2057 = LINE('',#11845,#2619) ;
#2058 = LINE('',#11848,#2620) ;
#2059 = LINE('',#11850,#2621) ;
#2060 = LINE('',#11851,#2622) ;
#2061 = LINE('',#11867,#2623) ;
#2062 = LINE('',#11875,#2624) ;
#2063 = LINE('',#11876,#2625) ;
#2064 = LINE('',#11879,#2626) ;
#2065 = LINE('',#11881,#2627) ;
#2066 = LINE('',#11882,#2628) ;
#2067 = LINE('',#11885,#2629) ;
#2068 = LINE('',#11891,#2630) ;
#2069 = LINE('',#11897,#2631) ;
#2070 = LINE('',#11901,#2632) ;
#2071 = LINE('',#11959,#2633) ;
#2072 = LINE('',#11963,#2634) ;
#2073 = LINE('',#11969,#2635) ;
#2074 = LINE('',#12320,#2636) ;
#2075 = LINE('',#12389,#2637) ;
#2076 = LINE('',#12442,#2638) ;
#2077 = LINE('',#12446,#2639) ;
#2078 = LINE('',#12504,#2640) ;
#2079 = LINE('',#12508,#2641) ;
#2080 = LINE('',#12514,#2642) ;
#2081 = LINE('',#12520,#2643) ;
#2082 = LINE('',#12523,#2644) ;
#2083 = LINE('',#12528,#2645) ;
#2084 = LINE('',#12531,#2646) ;
#2085 = LINE('',#12534,#2647) ;
#2086 = LINE('',#12536,#2648) ;
#2087 = LINE('',#12537,#2649) ;
#2088 = LINE('',#12540,#2650) ;
#2089 = LINE('',#12541,#2651) ;
#2090 = LINE('',#12544,#2652) ;
#2091 = LINE('',#12545,#2653) ;
#2092 = LINE('',#12547,#2654) ;
#2093 = LINE('',#12551,#2655) ;
#2094 = LINE('',#12553,#2656) ;
#2095 = LINE('',#12554,#2657) ;
#2096 = LINE('',#12557,#2658) ;
#2097 = LINE('',#12558,#2659) ;
#2098 = LINE('',#12561,#2660) ;
#2099 = LINE('',#12562,#2661) ;
#2100 = LINE('',#12564,#2662) ;
#2101 = LINE('',#12568,#2663) ;
#2102 = LINE('',#12570,#2664) ;
#2103 = LINE('',#12571,#2665) ;
#2104 = LINE('',#12574,#2666) ;
#2105 = LINE('',#12575,#2667) ;
#2106 = LINE('',#12578,#2668) ;
#2107 = LINE('',#12579,#2669) ;
#2108 = LINE('',#12582,#2670) ;
#2109 = LINE('',#12583,#2671) ;
#2110 = LINE('',#12586,#2672) ;
#2111 = LINE('',#12587,#2673) ;
#2112 = LINE('',#12590,#2674) ;
#2113 = LINE('',#12591,#2675) ;
#2114 = LINE('',#12594,#2676) ;
#2115 = LINE('',#12595,#2677) ;
#2116 = LINE('',#12598,#2678) ;
#2117 = LINE('',#12599,#2679) ;
#2118 = LINE('',#12602,#2680) ;
#2119 = LINE('',#12603,#2681) ;
#2120 = LINE('',#12611,#2682) ;
#2121 = LINE('',#12622,#2683) ;
#2122 = LINE('',#12628,#2684) ;
#2123 = LINE('',#12629,#2685) ;
#2124 = LINE('',#12632,#2686) ;
#2125 = LINE('',#12633,#2687) ;
#2126 = LINE('',#12636,#2688) ;
#2127 = LINE('',#12637,#2689) ;
#2128 = LINE('',#12639,#2690) ;
#2129 = LINE('',#12648,#2691) ;
#2130 = LINE('',#12653,#2692) ;
#2131 = LINE('',#12656,#2693) ;
#2132 = LINE('',#12657,#2694) ;
#2133 = LINE('',#12660,#2695) ;
#2134 = LINE('',#12661,#2696) ;
#2135 = LINE('',#12664,#2697) ;
#2136 = LINE('',#12665,#2698) ;
#2137 = LINE('',#12676,#2699) ;
#2138 = LINE('',#12687,#2700) ;
#2139 = LINE('',#12698,#2701) ;
#2140 = LINE('',#12709,#2702) ;
#2141 = LINE('',#12720,#2703) ;
#2142 = LINE('',#12728,#2704) ;
#2143 = LINE('',#12739,#2705) ;
#2144 = LINE('',#12750,#2706) ;
#2145 = LINE('',#12761,#2707) ;
#2146 = LINE('',#12772,#2708) ;
#2147 = LINE('',#12778,#2709) ;
#2148 = LINE('',#12779,#2710) ;
#2149 = LINE('',#12782,#2711) ;
#2150 = LINE('',#12783,#2712) ;
#2151 = LINE('',#12785,#2713) ;
#2152 = LINE('',#12794,#2714) ;
#2153 = LINE('',#12799,#2715) ;
#2154 = LINE('',#12810,#2716) ;
#2155 = LINE('',#12821,#2717) ;
#2156 = LINE('',#12824,#2718) ;
#2157 = LINE('',#12825,#2719) ;
#2158 = LINE('',#12836,#2720) ;
#2159 = LINE('',#12847,#2721) ;
#2160 = LINE('',#12858,#2722) ;
#2161 = LINE('',#12869,#2723) ;
#2162 = LINE('',#12880,#2724) ;
#2163 = LINE('',#12891,#2725) ;
#2164 = LINE('',#12902,#2726) ;
#2165 = LINE('',#12913,#2727) ;
#2166 = LINE('',#12924,#2728) ;
#2167 = LINE('',#12935,#2729) ;
#2168 = LINE('',#12946,#2730) ;
#2169 = LINE('',#12957,#2731) ;
#2170 = LINE('',#12968,#2732) ;
#2171 = LINE('',#12979,#2733) ;
#2172 = LINE('',#12987,#2734) ;
#2173 = LINE('',#12998,#2735) ;
#2174 = LINE('',#13009,#2736) ;
#2175 = LINE('',#13020,#2737) ;
#2176 = LINE('',#13031,#2738) ;
#2177 = LINE('',#13042,#2739) ;
#2178 = LINE('',#13053,#2740) ;
#2179 = LINE('',#13064,#2741) ;
#2180 = LINE('',#13075,#2742) ;
#2181 = LINE('',#13086,#2743) ;
#2182 = LINE('',#13097,#2744) ;
#2183 = LINE('',#13108,#2745) ;
#2184 = LINE('',#13119,#2746) ;
#2185 = LINE('',#13130,#2747) ;
#2186 = LINE('',#13141,#2748) ;
#2187 = LINE('',#13147,#2749) ;
#2188 = LINE('',#13148,#2750) ;
#2189 = LINE('',#13161,#2751) ;
#2190 = LINE('',#13163,#2752) ;
#2191 = LINE('',#13164,#2753) ;
#2192 = LINE('',#13167,#2754) ;
#2193 = LINE('',#13168,#2755) ;
#2194 = LINE('',#13171,#2756) ;
#2195 = LINE('',#13172,#2757) ;
#2196 = LINE('',#13175,#2758) ;
#2197 = LINE('',#13176,#2759) ;
#2198 = LINE('',#13179,#2760) ;
#2199 = LINE('',#13180,#2761) ;
#2200 = LINE('',#13183,#2762) ;
#2201 = LINE('',#13184,#2763) ;
#2202 = LINE('',#13187,#2764) ;
#2203 = LINE('',#13188,#2765) ;
#2204 = LINE('',#13191,#2766) ;
#2205 = LINE('',#13192,#2767) ;
#2206 = LINE('',#13195,#2768) ;
#2207 = LINE('',#13196,#2769) ;
#2208 = LINE('',#13204,#2770) ;
#2209 = LINE('',#13215,#2771) ;
#2210 = LINE('',#13221,#2772) ;
#2211 = LINE('',#13222,#2773) ;
#2212 = LINE('',#13225,#2774) ;
#2213 = LINE('',#13226,#2775) ;
#2214 = LINE('',#13229,#2776) ;
#2215 = LINE('',#13230,#2777) ;
#2216 = LINE('',#13232,#2778) ;
#2217 = LINE('',#13238,#2779) ;
#2218 = LINE('',#13248,#2780) ;
#2219 = LINE('',#13254,#2781) ;
#2220 = LINE('',#13330,#2782) ;
#2221 = LINE('',#13334,#2783) ;
#2222 = LINE('',#13339,#2784) ;
#2223 = LINE('',#13373,#2785) ;
#2224 = LINE('',#13377,#2786) ;
#2225 = LINE('',#13382,#2787) ;
#2226 = LINE('',#13416,#2788) ;
#2227 = LINE('',#13420,#2789) ;
#2228 = LINE('',#13425,#2790) ;
#2229 = LINE('',#13459,#2791) ;
#2230 = LINE('',#13475,#2792) ;
#2231 = LINE('',#13479,#2793) ;
#2232 = LINE('',#13483,#2794) ;
#2233 = LINE('',#13487,#2795) ;
#2234 = LINE('',#13492,#2796) ;
#2235 = LINE('',#13496,#2797) ;
#2236 = LINE('',#13501,#2798) ;
#2237 = LINE('',#13505,#2799) ;
#2238 = LINE('',#13510,#2800) ;
#2239 = LINE('',#13514,#2801) ;
#2240 = LINE('',#13519,#2802) ;
#2241 = LINE('',#13523,#2803) ;
#2242 = LINE('',#13544,#2804) ;
#2243 = LINE('',#13552,#2805) ;
#2244 = LINE('',#13560,#2806) ;
#2245 = LINE('',#13568,#2807) ;
#2246 = LINE('',#13576,#2808) ;
#2247 = LINE('',#13580,#2809) ;
#2248 = LINE('',#13588,#2810) ;
#2249 = LINE('',#13592,#2811) ;
#2250 = LINE('',#13594,#2812) ;
#2251 = LINE('',#13598,#2813) ;
#2252 = LINE('',#13601,#2814) ;
#2253 = LINE('',#13606,#2815) ;
#2254 = LINE('',#13608,#2816) ;
#2255 = LINE('',#13610,#2817) ;
#2256 = LINE('',#13611,#2818) ;
#2257 = LINE('',#13617,#2819) ;
#2258 = LINE('',#13620,#2820) ;
#2259 = LINE('',#13622,#2821) ;
#2260 = LINE('',#13623,#2822) ;
#2261 = LINE('',#13630,#2823) ;
#2262 = LINE('',#13632,#2824) ;
#2263 = LINE('',#13634,#2825) ;
#2264 = LINE('',#13635,#2826) ;
#2265 = LINE('',#13641,#2827) ;
#2266 = LINE('',#13644,#2828) ;
#2267 = LINE('',#13646,#2829) ;
#2268 = LINE('',#13647,#2830) ;
#2269 = LINE('',#13654,#2831) ;
#2270 = LINE('',#13656,#2832) ;
#2271 = LINE('',#13658,#2833) ;
#2272 = LINE('',#13659,#2834) ;
#2273 = LINE('',#13665,#2835) ;
#2274 = LINE('',#13668,#2836) ;
#2275 = LINE('',#13670,#2837) ;
#2276 = LINE('',#13671,#2838) ;
#2277 = LINE('',#13678,#2839) ;
#2278 = LINE('',#13680,#2840) ;
#2279 = LINE('',#13682,#2841) ;
#2280 = LINE('',#13683,#2842) ;
#2281 = LINE('',#13689,#2843) ;
#2282 = LINE('',#13692,#2844) ;
#2283 = LINE('',#13694,#2845) ;
#2284 = LINE('',#13695,#2846) ;
#2285 = LINE('',#13703,#2847) ;
#2286 = LINE('',#13711,#2848) ;
#2287 = LINE('',#13722,#2849) ;
#2288 = LINE('',#13746,#2850) ;
#2289 = LINE('',#13794,#2851) ;
#2290 = LINE('',#13842,#2852) ;
#2291 = LINE('',#13896,#2853) ;
#2292 = LINE('',#13944,#2854) ;
#2293 = LINE('',#13992,#2855) ;
#2294 = LINE('',#14046,#2856) ;
#2295 = LINE('',#14094,#2857) ;
#2296 = LINE('',#14142,#2858) ;
#2297 = LINE('',#14190,#2859) ;
#2298 = LINE('',#14244,#2860) ;
#2299 = LINE('',#14292,#2861) ;
#2300 = LINE('',#14340,#2862) ;
#2301 = LINE('',#14393,#2863) ;
#2302 = LINE('',#14414,#2864) ;
#2303 = LINE('',#14439,#2865) ;
#2304 = LINE('',#14463,#2866) ;
#2305 = LINE('',#14488,#2867) ;
#2306 = LINE('',#14513,#2868) ;
#2307 = LINE('',#14537,#2869) ;
#2308 = LINE('',#14561,#2870) ;
#2309 = LINE('',#14586,#2871) ;
#2310 = LINE('',#14611,#2872) ;
#2311 = LINE('',#14635,#2873) ;
#2312 = LINE('',#14660,#2874) ;
#2313 = LINE('',#14685,#2875) ;
#2314 = LINE('',#15813,#2876) ;
#2315 = LINE('',#15823,#2877) ;
#2316 = LINE('',#15825,#2878) ;
#2317 = LINE('',#15826,#2879) ;
#2318 = LINE('',#15830,#2880) ;
#2319 = LINE('',#15836,#2881) ;
#2320 = LINE('',#15841,#2882) ;
#2321 = LINE('',#15845,#2883) ;
#2322 = LINE('',#15849,#2884) ;
#2323 = LINE('',#15853,#2885) ;
#2324 = LINE('',#15857,#2886) ;
#2325 = LINE('',#15861,#2887) ;
#2326 = LINE('',#15865,#2888) ;
#2327 = LINE('',#15869,#2889) ;
#2328 = LINE('',#15873,#2890) ;
#2329 = LINE('',#15877,#2891) ;
#2330 = LINE('',#15881,#2892) ;
#2331 = LINE('',#15885,#2893) ;
#2332 = LINE('',#15889,#2894) ;
#2333 = LINE('',#15893,#2895) ;
#2334 = LINE('',#15897,#2896) ;
#2335 = LINE('',#15901,#2897) ;
#2336 = LINE('',#15905,#2898) ;
#2337 = LINE('',#15909,#2899) ;
#2338 = LINE('',#15913,#2900) ;
#2339 = LINE('',#15917,#2901) ;
#2340 = LINE('',#15921,#2902) ;
#2341 = LINE('',#15925,#2903) ;
#2342 = LINE('',#15929,#2904) ;
#2343 = LINE('',#15933,#2905) ;
#2344 = LINE('',#15937,#2906) ;
#2345 = LINE('',#15941,#2907) ;
#2346 = LINE('',#15945,#2908) ;
#2347 = LINE('',#15949,#2909) ;
#2348 = LINE('',#15953,#2910) ;
#2349 = LINE('',#15957,#2911) ;
#2350 = LINE('',#15961,#2912) ;
#2351 = LINE('',#15965,#2913) ;
#2352 = LINE('',#15969,#2914) ;
#2353 = LINE('',#15973,#2915) ;
#2354 = LINE('',#15977,#2916) ;
#2355 = LINE('',#15981,#2917) ;
#2356 = LINE('',#15985,#2918) ;
#2357 = LINE('',#15989,#2919) ;
#2358 = LINE('',#15993,#2920) ;
#2359 = LINE('',#15997,#2921) ;
#2360 = LINE('',#16001,#2922) ;
#2361 = LINE('',#16005,#2923) ;
#2362 = LINE('',#16009,#2924) ;
#2363 = LINE('',#16013,#2925) ;
#2364 = LINE('',#16017,#2926) ;
#2365 = LINE('',#16021,#2927) ;
#2366 = LINE('',#16025,#2928) ;
#2367 = LINE('',#16029,#2929) ;
#2368 = LINE('',#16033,#2930) ;
#2369 = LINE('',#16037,#2931) ;
#2370 = LINE('',#16041,#2932) ;
#2371 = LINE('',#16045,#2933) ;
#2372 = LINE('',#16049,#2934) ;
#2373 = LINE('',#16053,#2935) ;
#2374 = LINE('',#16057,#2936) ;
#2375 = LINE('',#16061,#2937) ;
#2376 = LINE('',#16066,#2938) ;
#2377 = LINE('',#16070,#2939) ;
#2378 = LINE('',#16074,#2940) ;
#2379 = LINE('',#16078,#2941) ;
#2380 = LINE('',#16082,#2942) ;
#2381 = LINE('',#16086,#2943) ;
#2382 = LINE('',#16090,#2944) ;
#2383 = LINE('',#16094,#2945) ;
#2384 = LINE('',#16098,#2946) ;
#2385 = LINE('',#16102,#2947) ;
#2386 = LINE('',#16106,#2948) ;
#2387 = LINE('',#16110,#2949) ;
#2388 = LINE('',#16114,#2950) ;
#2389 = LINE('',#16118,#2951) ;
#2390 = LINE('',#16122,#2952) ;
#2391 = LINE('',#16130,#2953) ;
#2392 = LINE('',#16131,#2954) ;
#2393 = LINE('',#16133,#2955) ;
#2394 = LINE('',#16144,#2956) ;
#2395 = LINE('',#16145,#2957) ;
#2396 = LINE('',#16147,#2958) ;
#2397 = LINE('',#16158,#2959) ;
#2398 = LINE('',#16159,#2960) ;
#2399 = LINE('',#16161,#2961) ;
#2400 = LINE('',#16172,#2962) ;
#2401 = LINE('',#16173,#2963) ;
#2402 = LINE('',#16175,#2964) ;
#2403 = LINE('',#16186,#2965) ;
#2404 = LINE('',#16187,#2966) ;
#2405 = LINE('',#16189,#2967) ;
#2406 = LINE('',#16200,#2968) ;
#2407 = LINE('',#16201,#2969) ;
#2408 = LINE('',#16203,#2970) ;
#2409 = LINE('',#16214,#2971) ;
#2410 = LINE('',#16215,#2972) ;
#2411 = LINE('',#16217,#2973) ;
#2412 = LINE('',#16228,#2974) ;
#2413 = LINE('',#16229,#2975) ;
#2414 = LINE('',#16231,#2976) ;
#2415 = LINE('',#16242,#2977) ;
#2416 = LINE('',#16243,#2978) ;
#2417 = LINE('',#16245,#2979) ;
#2418 = LINE('',#16256,#2980) ;
#2419 = LINE('',#16257,#2981) ;
#2420 = LINE('',#16259,#2982) ;
#2421 = LINE('',#16270,#2983) ;
#2422 = LINE('',#16271,#2984) ;
#2423 = LINE('',#16273,#2985) ;
#2424 = LINE('',#16284,#2986) ;
#2425 = LINE('',#16285,#2987) ;
#2426 = LINE('',#16287,#2988) ;
#2427 = LINE('',#16298,#2989) ;
#2428 = LINE('',#16299,#2990) ;
#2429 = LINE('',#16301,#2991) ;
#2430 = LINE('',#16312,#2992) ;
#2431 = LINE('',#16313,#2993) ;
#2432 = LINE('',#16315,#2994) ;
#2433 = LINE('',#16326,#2995) ;
#2434 = LINE('',#16327,#2996) ;
#2435 = LINE('',#16329,#2997) ;
#2436 = LINE('',#16340,#2998) ;
#2437 = LINE('',#16341,#2999) ;
#2438 = LINE('',#16343,#3000) ;
#2439 = LINE('',#16354,#3001) ;
#2440 = LINE('',#16355,#3002) ;
#2441 = LINE('',#16357,#3003) ;
#2442 = LINE('',#16368,#3004) ;
#2443 = LINE('',#16369,#3005) ;
#2444 = LINE('',#16371,#3006) ;
#2445 = LINE('',#16382,#3007) ;
#2446 = LINE('',#16383,#3008) ;
#2447 = LINE('',#16385,#3009) ;
#2448 = LINE('',#16396,#3010) ;
#2449 = LINE('',#16397,#3011) ;
#2450 = LINE('',#16399,#3012) ;
#2451 = LINE('',#16410,#3013) ;
#2452 = LINE('',#16411,#3014) ;
#2453 = LINE('',#16413,#3015) ;
#2454 = LINE('',#16424,#3016) ;
#2455 = LINE('',#16425,#3017) ;
#2456 = LINE('',#16427,#3018) ;
#2457 = LINE('',#16438,#3019) ;
#2458 = LINE('',#16439,#3020) ;
#2459 = LINE('',#16441,#3021) ;
#2460 = LINE('',#16452,#3022) ;
#2461 = LINE('',#16453,#3023) ;
#2462 = LINE('',#16455,#3024) ;
#2463 = LINE('',#16466,#3025) ;
#2464 = LINE('',#16467,#3026) ;
#2465 = LINE('',#16469,#3027) ;
#2466 = LINE('',#16480,#3028) ;
#2467 = LINE('',#16481,#3029) ;
#2468 = LINE('',#16483,#3030) ;
#2469 = LINE('',#16494,#3031) ;
#2470 = LINE('',#16495,#3032) ;
#2471 = LINE('',#16497,#3033) ;
#2472 = LINE('',#16508,#3034) ;
#2473 = LINE('',#16509,#3035) ;
#2474 = LINE('',#16511,#3036) ;
#2475 = LINE('',#16522,#3037) ;
#2476 = LINE('',#16523,#3038) ;
#2477 = LINE('',#16525,#3039) ;
#2478 = LINE('',#16536,#3040) ;
#2479 = LINE('',#16537,#3041) ;
#2480 = LINE('',#16539,#3042) ;
#2481 = LINE('',#16550,#3043) ;
#2482 = LINE('',#16551,#3044) ;
#2483 = LINE('',#16553,#3045) ;
#2484 = LINE('',#16564,#3046) ;
#2485 = LINE('',#16565,#3047) ;
#2486 = LINE('',#16567,#3048) ;
#2487 = LINE('',#16578,#3049) ;
#2488 = LINE('',#16579,#3050) ;
#2489 = LINE('',#16581,#3051) ;
#2490 = LINE('',#16592,#3052) ;
#2491 = LINE('',#16593,#3053) ;
#2492 = LINE('',#16595,#3054) ;
#2493 = LINE('',#16606,#3055) ;
#2494 = LINE('',#16607,#3056) ;
#2495 = LINE('',#16609,#3057) ;
#2496 = LINE('',#16619,#3058) ;
#2497 = LINE('',#16675,#3059) ;
#2498 = LINE('',#16687,#3060) ;
#2499 = LINE('',#16689,#3061) ;
#2500 = LINE('',#16693,#3062) ;
#2501 = LINE('',#16696,#3063) ;
#2502 = LINE('',#16699,#3064) ;
#2503 = LINE('',#16701,#3065) ;
#2504 = LINE('',#16705,#3066) ;
#2505 = LINE('',#16708,#3067) ;
#2506 = LINE('',#16711,#3068) ;
#2507 = LINE('',#16713,#3069) ;
#2508 = LINE('',#16717,#3070) ;
#2509 = LINE('',#16720,#3071) ;
#2510 = LINE('',#16722,#3072) ;
#2511 = LINE('',#16724,#3073) ;
#2512 = LINE('',#16726,#3074) ;
#2513 = LINE('',#16727,#3075) ;
#2514 = LINE('',#16729,#3076) ;
#2515 = LINE('',#16731,#3077) ;
#2516 = LINE('',#16732,#3078) ;
#2517 = LINE('',#16734,#3079) ;
#2518 = LINE('',#16736,#3080) ;
#2519 = LINE('',#16737,#3081) ;
#2520 = LINE('',#16741,#3082) ;
#2521 = LINE('',#16744,#3083) ;
#2522 = LINE('',#16746,#3084) ;
#2523 = LINE('',#16750,#3085) ;
#2524 = LINE('',#16753,#3086) ;
#2525 = LINE('',#16762,#3087) ;
#2526 = LINE('',#16766,#3088) ;
#2527 = LINE('',#16768,#3089) ;
#2528 = LINE('',#16769,#3090) ;
#2529 = LINE('',#16781,#3091) ;
#2530 = LINE('',#16787,#3092) ;
#2531 = LINE('',#16791,#3093) ;
#2532 = LINE('',#16795,#3094) ;
#2533 = LINE('',#16799,#3095) ;
#2534 = LINE('',#16803,#3096) ;
#2535 = LINE('',#16806,#3097) ;
#2536 = LINE('',#16812,#3098) ;
#2537 = LINE('',#16817,#3099) ;
#2538 = LINE('',#16819,#3100) ;
#2539 = LINE('',#16821,#3101) ;
#2540 = LINE('',#16822,#3102) ;
#2541 = LINE('',#16825,#3103) ;
#2542 = LINE('',#16827,#3104) ;
#2543 = LINE('',#16828,#3105) ;
#2544 = LINE('',#16831,#3106) ;
#2545 = LINE('',#16833,#3107) ;
#2546 = LINE('',#16834,#3108) ;
#2547 = LINE('',#16839,#3109) ;
#2548 = LINE('',#16841,#3110) ;
#2549 = LINE('',#16843,#3111) ;
#2550 = LINE('',#16850,#3112) ;
#2551 = LINE('',#16853,#3113) ;
#2552 = LINE('',#16855,#3114) ;
#2553 = LINE('',#16856,#3115) ;
#2554 = LINE('',#16859,#3116) ;
#2555 = LINE('',#16860,#3117) ;
#2556 = LINE('',#16865,#3118) ;
#2557 = LINE('',#16866,#3119) ;
#2558 = VECTOR('',#8980,4.3) ;
#2559 = VECTOR('',#8985,4.05) ;
#2560 = VECTOR('',#8996,2.025) ;
#2561 = VECTOR('',#9001,4.3) ;
#2562 = VECTOR('',#9006,4.05) ;
#2563 = VECTOR('',#9017,4.05) ;
#2564 = VECTOR('',#9022,10.) ;
#2565 = VECTOR('',#9027,10.) ;
#2566 = VECTOR('',#9028,10.) ;
#2567 = VECTOR('',#9029,10.) ;
#2568 = VECTOR('',#9040,10.) ;
#2569 = VECTOR('',#9043,10.) ;
#2570 = VECTOR('',#9044,10.) ;
#2571 = VECTOR('',#9045,10.) ;
#2572 = VECTOR('',#9054,10.) ;
#2573 = VECTOR('',#9057,10.) ;
#2574 = VECTOR('',#9062,10.) ;
#2575 = VECTOR('',#9065,10.) ;
#2576 = VECTOR('',#9068,10.) ;
#2577 = VECTOR('',#9071,10.) ;
#2578 = VECTOR('',#9076,10.) ;
#2579 = VECTOR('',#9079,10.) ;
#2580 = VECTOR('',#9146,5.75) ;
#2581 = VECTOR('',#9149,6.) ;
#2582 = VECTOR('',#9158,6.) ;
#2583 = VECTOR('',#9159,6.) ;
#2584 = VECTOR('',#9162,5.75) ;
#2585 = VECTOR('',#9165,10.) ;
#2586 = VECTOR('',#9166,10.) ;
#2587 = VECTOR('',#9167,10.) ;
#2588 = VECTOR('',#9168,10.) ;
#2589 = VECTOR('',#9169,10.) ;
#2590 = VECTOR('',#9170,10.) ;
#2591 = VECTOR('',#9171,10.) ;
#2592 = VECTOR('',#9172,10.) ;
#2593 = VECTOR('',#9173,10.) ;
#2594 = VECTOR('',#9174,10.) ;
#2595 = VECTOR('',#9175,10.) ;
#2596 = VECTOR('',#9176,10.) ;
#2597 = VECTOR('',#9177,10.) ;
#2598 = VECTOR('',#9178,10.) ;
#2599 = VECTOR('',#9179,10.) ;
#2600 = VECTOR('',#9180,10.) ;
#2601 = VECTOR('',#9181,10.) ;
#2602 = VECTOR('',#9182,10.) ;
#2603 = VECTOR('',#9183,10.) ;
#2604 = VECTOR('',#9184,10.) ;
#2605 = VECTOR('',#9185,10.) ;
#2606 = VECTOR('',#9186,10.) ;
#2607 = VECTOR('',#9187,10.) ;
#2608 = VECTOR('',#9188,10.) ;
#2609 = VECTOR('',#9189,10.) ;
#2610 = VECTOR('',#9190,10.) ;
#2611 = VECTOR('',#9191,10.) ;
#2612 = VECTOR('',#9196,10.) ;
#2613 = VECTOR('',#9197,10.) ;
#2614 = VECTOR('',#9200,10.) ;
#2615 = VECTOR('',#9201,10.) ;
#2616 = VECTOR('',#9206,10.) ;
#2617 = VECTOR('',#9207,10.) ;
#2618 = VECTOR('',#9208,10.) ;
#2619 = VECTOR('',#9209,10.) ;
#2620 = VECTOR('',#9212,10.) ;
#2621 = VECTOR('',#9213,10.) ;
#2622 = VECTOR('',#9214,10.) ;
#2623 = VECTOR('',#9215,10.) ;
#2624 = VECTOR('',#9220,10.) ;
#2625 = VECTOR('',#9221,10.) ;
#2626 = VECTOR('',#9224,10.) ;
#2627 = VECTOR('',#9225,10.) ;
#2628 = VECTOR('',#9226,10.) ;
#2629 = VECTOR('',#9231,10.) ;
#2630 = VECTOR('',#9238,15.5) ;
#2631 = VECTOR('',#9243,10.) ;
#2632 = VECTOR('',#9246,10.) ;
#2633 = VECTOR('',#9251,10.) ;
#2634 = VECTOR('',#9254,10.) ;
#2635 = VECTOR('',#9259,10.) ;
#2636 = VECTOR('',#9268,10.) ;
#2637 = VECTOR('',#9273,10.) ;
#2638 = VECTOR('',#9278,10.) ;
#2639 = VECTOR('',#9281,10.) ;
#2640 = VECTOR('',#9286,10.) ;
#2641 = VECTOR('',#9289,10.) ;
#2642 = VECTOR('',#9294,10.) ;
#2643 = VECTOR('',#9299,10.) ;
#2644 = VECTOR('',#9302,10.) ;
#2645 = VECTOR('',#9305,10.) ;
#2646 = VECTOR('',#9308,10.) ;
#2647 = VECTOR('',#9311,10.) ;
#2648 = VECTOR('',#9312,10.) ;
#2649 = VECTOR('',#9313,10.) ;
#2650 = VECTOR('',#9316,10.) ;
#2651 = VECTOR('',#9317,10.) ;
#2652 = VECTOR('',#9320,10.) ;
#2653 = VECTOR('',#9321,10.) ;
#2654 = VECTOR('',#9324,10.) ;
#2655 = VECTOR('',#9329,10.) ;
#2656 = VECTOR('',#9330,10.) ;
#2657 = VECTOR('',#9331,10.) ;
#2658 = VECTOR('',#9334,10.) ;
#2659 = VECTOR('',#9335,10.) ;
#2660 = VECTOR('',#9338,10.) ;
#2661 = VECTOR('',#9339,10.) ;
#2662 = VECTOR('',#9342,10.) ;
#2663 = VECTOR('',#9347,10.) ;
#2664 = VECTOR('',#9348,10.) ;
#2665 = VECTOR('',#9349,10.) ;
#2666 = VECTOR('',#9352,10.) ;
#2667 = VECTOR('',#9353,10.) ;
#2668 = VECTOR('',#9356,10.) ;
#2669 = VECTOR('',#9357,10.) ;
#2670 = VECTOR('',#9360,10.) ;
#2671 = VECTOR('',#9361,10.) ;
#2672 = VECTOR('',#9364,10.) ;
#2673 = VECTOR('',#9365,10.) ;
#2674 = VECTOR('',#9368,10.) ;
#2675 = VECTOR('',#9369,10.) ;
#2676 = VECTOR('',#9372,10.) ;
#2677 = VECTOR('',#9373,10.) ;
#2678 = VECTOR('',#9376,10.) ;
#2679 = VECTOR('',#9377,10.) ;
#2680 = VECTOR('',#9380,10.) ;
#2681 = VECTOR('',#9381,10.) ;
#2682 = VECTOR('',#9382,10.) ;
#2683 = VECTOR('',#9383,10.) ;
#2684 = VECTOR('',#9386,10.) ;
#2685 = VECTOR('',#9387,10.) ;
#2686 = VECTOR('',#9390,10.) ;
#2687 = VECTOR('',#9391,10.) ;
#2688 = VECTOR('',#9394,10.) ;
#2689 = VECTOR('',#9395,10.) ;
#2690 = VECTOR('',#9398,10.) ;
#2691 = VECTOR('',#9401,10.) ;
#2692 = VECTOR('',#9402,10.) ;
#2693 = VECTOR('',#9405,10.) ;
#2694 = VECTOR('',#9406,10.) ;
#2695 = VECTOR('',#9409,10.) ;
#2696 = VECTOR('',#9410,10.) ;
#2697 = VECTOR('',#9413,10.) ;
#2698 = VECTOR('',#9414,10.) ;
#2699 = VECTOR('',#9415,10.) ;
#2700 = VECTOR('',#9416,10.) ;
#2701 = VECTOR('',#9417,10.) ;
#2702 = VECTOR('',#9418,10.) ;
#2703 = VECTOR('',#9419,10.) ;
#2704 = VECTOR('',#9420,10.) ;
#2705 = VECTOR('',#9421,10.) ;
#2706 = VECTOR('',#9422,10.) ;
#2707 = VECTOR('',#9423,10.) ;
#2708 = VECTOR('',#9424,10.) ;
#2709 = VECTOR('',#9427,10.) ;
#2710 = VECTOR('',#9428,10.) ;
#2711 = VECTOR('',#9431,10.) ;
#2712 = VECTOR('',#9432,10.) ;
#2713 = VECTOR('',#9435,10.) ;
#2714 = VECTOR('',#9438,10.) ;
#2715 = VECTOR('',#9439,10.) ;
#2716 = VECTOR('',#9440,10.) ;
#2717 = VECTOR('',#9441,10.) ;
#2718 = VECTOR('',#9444,10.) ;
#2719 = VECTOR('',#9445,10.) ;
#2720 = VECTOR('',#9446,10.) ;
#2721 = VECTOR('',#9447,10.) ;
#2722 = VECTOR('',#9448,10.) ;
#2723 = VECTOR('',#9449,10.) ;
#2724 = VECTOR('',#9450,10.) ;
#2725 = VECTOR('',#9451,10.) ;
#2726 = VECTOR('',#9452,10.) ;
#2727 = VECTOR('',#9453,10.) ;
#2728 = VECTOR('',#9454,10.) ;
#2729 = VECTOR('',#9455,10.) ;
#2730 = VECTOR('',#9456,10.) ;
#2731 = VECTOR('',#9457,10.) ;
#2732 = VECTOR('',#9458,10.) ;
#2733 = VECTOR('',#9459,10.) ;
#2734 = VECTOR('',#9460,10.) ;
#2735 = VECTOR('',#9461,10.) ;
#2736 = VECTOR('',#9462,10.) ;
#2737 = VECTOR('',#9463,10.) ;
#2738 = VECTOR('',#9464,10.) ;
#2739 = VECTOR('',#9465,10.) ;
#2740 = VECTOR('',#9466,10.) ;
#2741 = VECTOR('',#9467,10.) ;
#2742 = VECTOR('',#9468,10.) ;
#2743 = VECTOR('',#9469,10.) ;
#2744 = VECTOR('',#9470,10.) ;
#2745 = VECTOR('',#9471,10.) ;
#2746 = VECTOR('',#9472,10.) ;
#2747 = VECTOR('',#9473,10.) ;
#2748 = VECTOR('',#9474,10.) ;
#2749 = VECTOR('',#9477,10.) ;
#2750 = VECTOR('',#9478,10.) ;
#2751 = VECTOR('',#9483,10.) ;
#2752 = VECTOR('',#9484,10.) ;
#2753 = VECTOR('',#9485,10.) ;
#2754 = VECTOR('',#9488,10.) ;
#2755 = VECTOR('',#9489,10.) ;
#2756 = VECTOR('',#9492,10.) ;
#2757 = VECTOR('',#9493,10.) ;
#2758 = VECTOR('',#9496,10.) ;
#2759 = VECTOR('',#9497,10.) ;
#2760 = VECTOR('',#9500,10.) ;
#2761 = VECTOR('',#9501,10.) ;
#2762 = VECTOR('',#9504,10.) ;
#2763 = VECTOR('',#9505,10.) ;
#2764 = VECTOR('',#9508,10.) ;
#2765 = VECTOR('',#9509,10.) ;
#2766 = VECTOR('',#9512,10.) ;
#2767 = VECTOR('',#9513,10.) ;
#2768 = VECTOR('',#9516,10.) ;
#2769 = VECTOR('',#9517,10.) ;
#2770 = VECTOR('',#9518,10.) ;
#2771 = VECTOR('',#9519,10.) ;
#2772 = VECTOR('',#9522,10.) ;
#2773 = VECTOR('',#9523,10.) ;
#2774 = VECTOR('',#9526,10.) ;
#2775 = VECTOR('',#9527,10.) ;
#2776 = VECTOR('',#9530,10.) ;
#2777 = VECTOR('',#9531,10.) ;
#2778 = VECTOR('',#9534,10.) ;
#2779 = VECTOR('',#9541,15.1) ;
#2780 = VECTOR('',#9554,10.) ;
#2781 = VECTOR('',#9559,10.) ;
#2782 = VECTOR('',#9582,4.) ;
#2783 = VECTOR('',#9587,10.) ;
#2784 = VECTOR('',#9592,10.) ;
#2785 = VECTOR('',#9597,4.) ;
#2786 = VECTOR('',#9602,10.) ;
#2787 = VECTOR('',#9607,10.) ;
#2788 = VECTOR('',#9612,4.) ;
#2789 = VECTOR('',#9617,10.) ;
#2790 = VECTOR('',#9622,10.) ;
#2791 = VECTOR('',#9627,4.) ;
#2792 = VECTOR('',#9648,2.25) ;
#2793 = VECTOR('',#9653,2.25) ;
#2794 = VECTOR('',#9658,2.25) ;
#2795 = VECTOR('',#9663,2.25) ;
#2796 = VECTOR('',#9668,10.) ;
#2797 = VECTOR('',#9671,10.) ;
#2798 = VECTOR('',#9676,10.) ;
#2799 = VECTOR('',#9679,10.) ;
#2800 = VECTOR('',#9684,10.) ;
#2801 = VECTOR('',#9687,10.) ;
#2802 = VECTOR('',#9692,10.) ;
#2803 = VECTOR('',#9695,10.) ;
#2804 = VECTOR('',#9732,15.5) ;
#2805 = VECTOR('',#9741,12.6) ;
#2806 = VECTOR('',#9752,12.) ;
#2807 = VECTOR('',#9761,12.6) ;
#2808 = VECTOR('',#9772,12.) ;
#2809 = VECTOR('',#9777,12.) ;
#2810 = VECTOR('',#9788,25.25) ;
#2811 = VECTOR('',#9793,25.5) ;
#2812 = VECTOR('',#9796,25.25) ;
#2813 = VECTOR('',#9801,15.25) ;
#2814 = VECTOR('',#9806,12.) ;
#2815 = VECTOR('',#9811,10.) ;
#2816 = VECTOR('',#9812,10.) ;
#2817 = VECTOR('',#9813,10.) ;
#2818 = VECTOR('',#9814,10.) ;
#2819 = VECTOR('',#9821,10.) ;
#2820 = VECTOR('',#9824,10.) ;
#2821 = VECTOR('',#9825,10.) ;
#2822 = VECTOR('',#9826,10.) ;
#2823 = VECTOR('',#9835,10.) ;
#2824 = VECTOR('',#9836,10.) ;
#2825 = VECTOR('',#9837,10.) ;
#2826 = VECTOR('',#9838,10.) ;
#2827 = VECTOR('',#9845,10.) ;
#2828 = VECTOR('',#9848,10.) ;
#2829 = VECTOR('',#9849,10.) ;
#2830 = VECTOR('',#9850,10.) ;
#2831 = VECTOR('',#9859,10.) ;
#2832 = VECTOR('',#9860,10.) ;
#2833 = VECTOR('',#9861,10.) ;
#2834 = VECTOR('',#9862,10.) ;
#2835 = VECTOR('',#9869,10.) ;
#2836 = VECTOR('',#9872,10.) ;
#2837 = VECTOR('',#9873,10.) ;
#2838 = VECTOR('',#9874,10.) ;
#2839 = VECTOR('',#9883,10.) ;
#2840 = VECTOR('',#9884,10.) ;
#2841 = VECTOR('',#9885,10.) ;
#2842 = VECTOR('',#9886,10.) ;
#2843 = VECTOR('',#9893,10.) ;
#2844 = VECTOR('',#9896,10.) ;
#2845 = VECTOR('',#9897,10.) ;
#2846 = VECTOR('',#9898,10.) ;
#2847 = VECTOR('',#9909,8.15) ;
#2848 = VECTOR('',#9920,8.5) ;
#2849 = VECTOR('',#9933,2.) ;
#2850 = VECTOR('',#9938,2.) ;
#2851 = VECTOR('',#9941,2.) ;
#2852 = VECTOR('',#9944,2.) ;
#2853 = VECTOR('',#9947,2.) ;
#2854 = VECTOR('',#9950,2.) ;
#2855 = VECTOR('',#9953,2.) ;
#2856 = VECTOR('',#9956,2.) ;
#2857 = VECTOR('',#9959,2.) ;
#2858 = VECTOR('',#9962,2.) ;
#2859 = VECTOR('',#9965,2.) ;
#2860 = VECTOR('',#9968,2.) ;
#2861 = VECTOR('',#9971,2.) ;
#2862 = VECTOR('',#9974,2.) ;
#2863 = VECTOR('',#9979,1.5555) ;
#2864 = VECTOR('',#9984,1.5555) ;
#2865 = VECTOR('',#9987,1.5555) ;
#2866 = VECTOR('',#9990,1.5555) ;
#2867 = VECTOR('',#9993,1.5555) ;
#2868 = VECTOR('',#9996,1.5555) ;
#2869 = VECTOR('',#9999,1.5555) ;
#2870 = VECTOR('',#10002,1.5555) ;
#2871 = VECTOR('',#10005,1.5555) ;
#2872 = VECTOR('',#10008,1.5555) ;
#2873 = VECTOR('',#10011,1.5555) ;
#2874 = VECTOR('',#10014,1.5555) ;
#2875 = VECTOR('',#10017,1.5555) ;
#2876 = VECTOR('',#10048,1.704) ;
#2877 = VECTOR('',#10055,10.) ;
#2878 = VECTOR('',#10056,10.) ;
#2879 = VECTOR('',#10057,10.) ;
#2880 = VECTOR('',#10062,10.) ;
#2881 = VECTOR('',#10065,10.) ;
#2882 = VECTOR('',#10070,10.) ;
#2883 = VECTOR('',#10073,10.) ;
#2884 = VECTOR('',#10076,10.) ;
#2885 = VECTOR('',#10079,10.) ;
#2886 = VECTOR('',#10082,10.) ;
#2887 = VECTOR('',#10085,10.) ;
#2888 = VECTOR('',#10088,10.) ;
#2889 = VECTOR('',#10091,10.) ;
#2890 = VECTOR('',#10094,10.) ;
#2891 = VECTOR('',#10097,10.) ;
#2892 = VECTOR('',#10100,10.) ;
#2893 = VECTOR('',#10103,10.) ;
#2894 = VECTOR('',#10106,10.) ;
#2895 = VECTOR('',#10109,10.) ;
#2896 = VECTOR('',#10112,10.) ;
#2897 = VECTOR('',#10115,10.) ;
#2898 = VECTOR('',#10118,10.) ;
#2899 = VECTOR('',#10121,10.) ;
#2900 = VECTOR('',#10124,10.) ;
#2901 = VECTOR('',#10127,10.) ;
#2902 = VECTOR('',#10130,10.) ;
#2903 = VECTOR('',#10133,10.) ;
#2904 = VECTOR('',#10136,10.) ;
#2905 = VECTOR('',#10139,10.) ;
#2906 = VECTOR('',#10142,10.) ;
#2907 = VECTOR('',#10145,10.) ;
#2908 = VECTOR('',#10148,10.) ;
#2909 = VECTOR('',#10151,10.) ;
#2910 = VECTOR('',#10154,10.) ;
#2911 = VECTOR('',#10157,10.) ;
#2912 = VECTOR('',#10160,10.) ;
#2913 = VECTOR('',#10163,10.) ;
#2914 = VECTOR('',#10166,10.) ;
#2915 = VECTOR('',#10169,10.) ;
#2916 = VECTOR('',#10172,10.) ;
#2917 = VECTOR('',#10175,10.) ;
#2918 = VECTOR('',#10178,10.) ;
#2919 = VECTOR('',#10181,10.) ;
#2920 = VECTOR('',#10184,10.) ;
#2921 = VECTOR('',#10187,10.) ;
#2922 = VECTOR('',#10190,10.) ;
#2923 = VECTOR('',#10193,10.) ;
#2924 = VECTOR('',#10196,10.) ;
#2925 = VECTOR('',#10199,10.) ;
#2926 = VECTOR('',#10202,10.) ;
#2927 = VECTOR('',#10205,10.) ;
#2928 = VECTOR('',#10208,10.) ;
#2929 = VECTOR('',#10211,10.) ;
#2930 = VECTOR('',#10214,10.) ;
#2931 = VECTOR('',#10217,10.) ;
#2932 = VECTOR('',#10220,10.) ;
#2933 = VECTOR('',#10223,10.) ;
#2934 = VECTOR('',#10226,10.) ;
#2935 = VECTOR('',#10229,10.) ;
#2936 = VECTOR('',#10232,10.) ;
#2937 = VECTOR('',#10235,3.5) ;
#2938 = VECTOR('',#10240,10.) ;
#2939 = VECTOR('',#10243,10.) ;
#2940 = VECTOR('',#10246,10.) ;
#2941 = VECTOR('',#10249,10.) ;
#2942 = VECTOR('',#10252,10.) ;
#2943 = VECTOR('',#10255,10.) ;
#2944 = VECTOR('',#10258,10.) ;
#2945 = VECTOR('',#10261,10.) ;
#2946 = VECTOR('',#10264,10.) ;
#2947 = VECTOR('',#10267,10.) ;
#2948 = VECTOR('',#10270,10.) ;
#2949 = VECTOR('',#10273,10.) ;
#2950 = VECTOR('',#10276,10.) ;
#2951 = VECTOR('',#10279,10.) ;
#2952 = VECTOR('',#10282,10.) ;
#2953 = VECTOR('',#10287,10.) ;
#2954 = VECTOR('',#10288,10.) ;
#2955 = VECTOR('',#10291,10.) ;
#2956 = VECTOR('',#10296,10.) ;
#2957 = VECTOR('',#10297,10.) ;
#2958 = VECTOR('',#10300,10.) ;
#2959 = VECTOR('',#10305,10.) ;
#2960 = VECTOR('',#10306,10.) ;
#2961 = VECTOR('',#10309,10.) ;
#2962 = VECTOR('',#10314,10.) ;
#2963 = VECTOR('',#10315,10.) ;
#2964 = VECTOR('',#10318,10.) ;
#2965 = VECTOR('',#10323,10.) ;
#2966 = VECTOR('',#10324,10.) ;
#2967 = VECTOR('',#10327,10.) ;
#2968 = VECTOR('',#10332,10.) ;
#2969 = VECTOR('',#10333,10.) ;
#2970 = VECTOR('',#10336,10.) ;
#2971 = VECTOR('',#10341,10.) ;
#2972 = VECTOR('',#10342,10.) ;
#2973 = VECTOR('',#10345,10.) ;
#2974 = VECTOR('',#10350,10.) ;
#2975 = VECTOR('',#10351,10.) ;
#2976 = VECTOR('',#10354,10.) ;
#2977 = VECTOR('',#10359,10.) ;
#2978 = VECTOR('',#10360,10.) ;
#2979 = VECTOR('',#10363,10.) ;
#2980 = VECTOR('',#10368,10.) ;
#2981 = VECTOR('',#10369,10.) ;
#2982 = VECTOR('',#10372,10.) ;
#2983 = VECTOR('',#10377,10.) ;
#2984 = VECTOR('',#10378,10.) ;
#2985 = VECTOR('',#10381,10.) ;
#2986 = VECTOR('',#10386,10.) ;
#2987 = VECTOR('',#10387,10.) ;
#2988 = VECTOR('',#10390,10.) ;
#2989 = VECTOR('',#10395,10.) ;
#2990 = VECTOR('',#10396,10.) ;
#2991 = VECTOR('',#10399,10.) ;
#2992 = VECTOR('',#10404,10.) ;
#2993 = VECTOR('',#10405,10.) ;
#2994 = VECTOR('',#10408,10.) ;
#2995 = VECTOR('',#10413,10.) ;
#2996 = VECTOR('',#10414,10.) ;
#2997 = VECTOR('',#10417,10.) ;
#2998 = VECTOR('',#10422,10.) ;
#2999 = VECTOR('',#10423,10.) ;
#3000 = VECTOR('',#10426,10.) ;
#3001 = VECTOR('',#10431,10.) ;
#3002 = VECTOR('',#10432,10.) ;
#3003 = VECTOR('',#10435,10.) ;
#3004 = VECTOR('',#10440,10.) ;
#3005 = VECTOR('',#10441,10.) ;
#3006 = VECTOR('',#10444,10.) ;
#3007 = VECTOR('',#10449,10.) ;
#3008 = VECTOR('',#10450,10.) ;
#3009 = VECTOR('',#10453,10.) ;
#3010 = VECTOR('',#10458,10.) ;
#3011 = VECTOR('',#10459,10.) ;
#3012 = VECTOR('',#10462,10.) ;
#3013 = VECTOR('',#10467,10.) ;
#3014 = VECTOR('',#10468,10.) ;
#3015 = VECTOR('',#10471,10.) ;
#3016 = VECTOR('',#10476,10.) ;
#3017 = VECTOR('',#10477,10.) ;
#3018 = VECTOR('',#10480,10.) ;
#3019 = VECTOR('',#10485,10.) ;
#3020 = VECTOR('',#10486,10.) ;
#3021 = VECTOR('',#10489,10.) ;
#3022 = VECTOR('',#10494,10.) ;
#3023 = VECTOR('',#10495,10.) ;
#3024 = VECTOR('',#10498,10.) ;
#3025 = VECTOR('',#10503,10.) ;
#3026 = VECTOR('',#10504,10.) ;
#3027 = VECTOR('',#10507,10.) ;
#3028 = VECTOR('',#10512,10.) ;
#3029 = VECTOR('',#10513,10.) ;
#3030 = VECTOR('',#10516,10.) ;
#3031 = VECTOR('',#10521,10.) ;
#3032 = VECTOR('',#10522,10.) ;
#3033 = VECTOR('',#10525,10.) ;
#3034 = VECTOR('',#10530,10.) ;
#3035 = VECTOR('',#10531,10.) ;
#3036 = VECTOR('',#10534,10.) ;
#3037 = VECTOR('',#10539,10.) ;
#3038 = VECTOR('',#10540,10.) ;
#3039 = VECTOR('',#10543,10.) ;
#3040 = VECTOR('',#10548,10.) ;
#3041 = VECTOR('',#10549,10.) ;
#3042 = VECTOR('',#10552,10.) ;
#3043 = VECTOR('',#10557,10.) ;
#3044 = VECTOR('',#10558,10.) ;
#3045 = VECTOR('',#10561,10.) ;
#3046 = VECTOR('',#10566,10.) ;
#3047 = VECTOR('',#10567,10.) ;
#3048 = VECTOR('',#10570,10.) ;
#3049 = VECTOR('',#10575,10.) ;
#3050 = VECTOR('',#10576,10.) ;
#3051 = VECTOR('',#10579,10.) ;
#3052 = VECTOR('',#10584,10.) ;
#3053 = VECTOR('',#10585,10.) ;
#3054 = VECTOR('',#10588,10.) ;
#3055 = VECTOR('',#10593,10.) ;
#3056 = VECTOR('',#10594,10.) ;
#3057 = VECTOR('',#10597,10.) ;
#3058 = VECTOR('',#10608,3.3) ;
#3059 = VECTOR('',#10625,1.83205080756888) ;
#3060 = VECTOR('',#10630,10.) ;
#3061 = VECTOR('',#10631,10.) ;
#3062 = VECTOR('',#10636,10.) ;
#3063 = VECTOR('',#10639,10.) ;
#3064 = VECTOR('',#10642,10.) ;
#3065 = VECTOR('',#10643,10.) ;
#3066 = VECTOR('',#10648,10.) ;
#3067 = VECTOR('',#10651,10.) ;
#3068 = VECTOR('',#10654,10.) ;
#3069 = VECTOR('',#10655,10.) ;
#3070 = VECTOR('',#10660,10.) ;
#3071 = VECTOR('',#10663,10.) ;
#3072 = VECTOR('',#10666,10.) ;
#3073 = VECTOR('',#10667,10.) ;
#3074 = VECTOR('',#10668,10.) ;
#3075 = VECTOR('',#10669,10.) ;
#3076 = VECTOR('',#10672,10.) ;
#3077 = VECTOR('',#10673,10.) ;
#3078 = VECTOR('',#10674,10.) ;
#3079 = VECTOR('',#10677,10.) ;
#3080 = VECTOR('',#10678,10.) ;
#3081 = VECTOR('',#10679,10.) ;
#3082 = VECTOR('',#10686,10.) ;
#3083 = VECTOR('',#10691,10.) ;
#3084 = VECTOR('',#10694,10.) ;
#3085 = VECTOR('',#10697,10.) ;
#3086 = VECTOR('',#10702,10.) ;
#3087 = VECTOR('',#10719,10.) ;
#3088 = VECTOR('',#10724,0.866025403784438) ;
#3089 = VECTOR('',#10727,10.) ;
#3090 = VECTOR('',#10728,10.) ;
#3091 = VECTOR('',#10745,12.) ;
#3092 = VECTOR('',#10752,8.625) ;
#3093 = VECTOR('',#10757,8.05) ;
#3094 = VECTOR('',#10762,8.325) ;
#3095 = VECTOR('',#10767,8.325) ;
#3096 = VECTOR('',#10772,8.05) ;
#3097 = VECTOR('',#10777,8.525) ;
#3098 = VECTOR('',#10784,0.85) ;
#3099 = VECTOR('',#10789,10.) ;
#3100 = VECTOR('',#10790,10.) ;
#3101 = VECTOR('',#10791,10.) ;
#3102 = VECTOR('',#10792,10.) ;
#3103 = VECTOR('',#10795,10.) ;
#3104 = VECTOR('',#10796,10.) ;
#3105 = VECTOR('',#10797,10.) ;
#3106 = VECTOR('',#10800,10.) ;
#3107 = VECTOR('',#10801,10.) ;
#3108 = VECTOR('',#10802,10.) ;
#3109 = VECTOR('',#10807,10.) ;
#3110 = VECTOR('',#10808,10.) ;
#3111 = VECTOR('',#10809,10.) ;
#3112 = VECTOR('',#10818,0.85) ;
#3113 = VECTOR('',#10821,10.) ;
#3114 = VECTOR('',#10822,10.) ;
#3115 = VECTOR('',#10823,10.) ;
#3116 = VECTOR('',#10826,10.) ;
#3117 = VECTOR('',#10827,10.) ;
#3118 = VECTOR('',#10834,10.) ;
#3119 = VECTOR('',#10835,10.) ;
#3120 = CIRCLE('',#8266,4.55) ;
#3121 = CIRCLE('',#8267,4.05) ;
#3122 = CIRCLE('',#8269,4.05) ;
#3123 = CIRCLE('',#8270,4.05) ;
#3124 = CIRCLE('',#8272,5.5) ;
#3125 = CIRCLE('',#8275,4.55) ;
#3126 = CIRCLE('',#8276,4.05) ;
#3127 = CIRCLE('',#8278,4.05) ;
#3128 = CIRCLE('',#8279,4.05) ;
#3129 = CIRCLE('',#8281,5.5) ;
#3130 = CIRCLE('',#8284,6.) ;
#3131 = CIRCLE('',#8285,6.) ;
#3132 = CIRCLE('',#8288,6.) ;
#3133 = CIRCLE('',#8289,6.) ;
#3134 = CIRCLE('',#8291,6.) ;
#3135 = CIRCLE('',#8294,6.) ;
#3136 = CIRCLE('',#8296,1.65) ;
#3137 = CIRCLE('',#8297,1.65) ;
#3138 = CIRCLE('',#8299,1.65) ;
#3139 = CIRCLE('',#8300,1.65) ;
#3140 = CIRCLE('',#8302,1.65) ;
#3141 = CIRCLE('',#8303,1.65) ;
#3142 = CIRCLE('',#8305,1.65) ;
#3143 = CIRCLE('',#8306,1.65) ;
#3144 = CIRCLE('',#8308,8.) ;
#3145 = CIRCLE('',#8309,7.7) ;
#3146 = CIRCLE('',#8311,8.) ;
#3147 = CIRCLE('',#8312,7.7) ;
#3148 = CIRCLE('',#8314,7.7) ;
#3149 = CIRCLE('',#8315,8.) ;
#3150 = CIRCLE('',#8317,8.) ;
#3151 = CIRCLE('',#8318,7.7) ;
#3152 = CIRCLE('',#8320,8.) ;
#3153 = CIRCLE('',#8322,8.) ;
#3154 = CIRCLE('',#8324,8.) ;
#3155 = CIRCLE('',#8326,8.) ;
#3156 = CIRCLE('',#8328,7.7) ;
#3157 = CIRCLE('',#8330,7.7) ;
#3158 = CIRCLE('',#8332,7.7) ;
#3159 = CIRCLE('',#8334,7.7) ;
#3160 = CIRCLE('',#8336,6.) ;
#3161 = CIRCLE('',#8338,6.) ;
#3162 = CIRCLE('',#8341,6.) ;
#3163 = CIRCLE('',#8343,6.) ;
#3164 = CIRCLE('',#8350,15.5) ;
#3165 = CIRCLE('',#8353,15.5) ;
#3166 = CIRCLE('',#8356,15.5) ;
#3167 = CIRCLE('',#8359,15.5) ;
#3168 = CIRCLE('',#8360,15.5) ;
#3169 = CIRCLE('',#8361,15.5) ;
#3170 = CIRCLE('',#8362,15.5) ;
#3171 = CIRCLE('',#8365,15.5) ;
#3172 = CIRCLE('',#8366,15.5) ;
#3173 = CIRCLE('',#8371,15.5) ;
#3174 = CIRCLE('',#8372,15.5) ;
#3175 = CIRCLE('',#8373,15.5) ;
#3176 = CIRCLE('',#8374,15.5) ;
#3177 = CIRCLE('',#8375,15.5) ;
#3178 = CIRCLE('',#8376,15.5) ;
#3179 = CIRCLE('',#8379,15.5) ;
#3180 = CIRCLE('',#8380,15.5) ;
#3181 = CIRCLE('',#8383,15.5) ;
#3182 = CIRCLE('',#8384,15.5) ;
#3183 = CIRCLE('',#8385,15.5) ;
#3184 = CIRCLE('',#8386,15.5) ;
#3185 = CIRCLE('',#8436,15.1) ;
#3186 = CIRCLE('',#8437,15.1) ;
#3187 = CIRCLE('',#8439,15.5) ;
#3188 = CIRCLE('',#8443,4.) ;
#3189 = CIRCLE('',#8444,4.) ;
#3190 = CIRCLE('',#8445,4.3) ;
#3191 = CIRCLE('',#8447,15.9) ;
#3192 = CIRCLE('',#8448,15.9) ;
#3193 = CIRCLE('',#8449,15.9) ;
#3194 = CIRCLE('',#8450,15.9) ;
#3195 = CIRCLE('',#8451,0.4) ;
#3196 = CIRCLE('',#8452,15.5) ;
#3197 = CIRCLE('',#8453,15.5) ;
#3198 = CIRCLE('',#8454,15.9) ;
#3199 = CIRCLE('',#8456,4.) ;
#3200 = CIRCLE('',#8458,4.) ;
#3201 = CIRCLE('',#8459,4.) ;
#3202 = CIRCLE('',#8460,4.3) ;
#3203 = CIRCLE('',#8462,4.) ;
#3204 = CIRCLE('',#8464,4.) ;
#3205 = CIRCLE('',#8465,4.) ;
#3206 = CIRCLE('',#8466,4.3) ;
#3207 = CIRCLE('',#8468,4.) ;
#3208 = CIRCLE('',#8470,4.) ;
#3209 = CIRCLE('',#8471,4.) ;
#3210 = CIRCLE('',#8472,4.3) ;
#3211 = CIRCLE('',#8474,4.) ;
#3212 = CIRCLE('',#8476,2.25) ;
#3213 = CIRCLE('',#8478,2.25) ;
#3214 = CIRCLE('',#8480,2.25) ;
#3215 = CIRCLE('',#8482,2.25) ;
#3216 = CIRCLE('',#8484,2.25) ;
#3217 = CIRCLE('',#8486,2.25) ;
#3218 = CIRCLE('',#8488,2.25) ;
#3219 = CIRCLE('',#8490,2.25) ;
#3220 = CIRCLE('',#8492,1.65) ;
#3221 = CIRCLE('',#8493,1.65) ;
#3222 = CIRCLE('',#8495,1.65) ;
#3223 = CIRCLE('',#8496,1.65) ;
#3224 = CIRCLE('',#8498,1.65) ;
#3225 = CIRCLE('',#8499,1.65) ;
#3226 = CIRCLE('',#8501,1.65) ;
#3227 = CIRCLE('',#8502,1.65) ;
#3228 = CIRCLE('',#8504,12.) ;
#3229 = CIRCLE('',#8505,8.6) ;
#3230 = CIRCLE('',#8506,8.6) ;
#3231 = CIRCLE('',#8507,8.6) ;
#3232 = CIRCLE('',#8508,8.6) ;
#3233 = CIRCLE('',#8510,8.6) ;
#3234 = CIRCLE('',#8512,8.6) ;
#3235 = CIRCLE('',#8514,8.6) ;
#3236 = CIRCLE('',#8516,8.6) ;
#3237 = CIRCLE('',#8518,25.) ;
#3238 = CIRCLE('',#8521,12.6) ;
#3239 = CIRCLE('',#8522,12.) ;
#3240 = CIRCLE('',#8524,12.6) ;
#3241 = CIRCLE('',#8526,12.) ;
#3242 = CIRCLE('',#8528,12.) ;
#3243 = CIRCLE('',#8530,12.6) ;
#3244 = CIRCLE('',#8531,12.) ;
#3245 = CIRCLE('',#8533,12.6) ;
#3246 = CIRCLE('',#8535,12.) ;
#3247 = CIRCLE('',#8537,12.) ;
#3248 = CIRCLE('',#8540,12.) ;
#3249 = CIRCLE('',#8542,25.) ;
#3250 = CIRCLE('',#8544,25.5) ;
#3251 = CIRCLE('',#8546,25.5) ;
#3252 = CIRCLE('',#8549,15.) ;
#3253 = CIRCLE('',#8555,8.15) ;
#3254 = CIRCLE('',#8556,8.5) ;
#3255 = CIRCLE('',#8559,8.15) ;
#3256 = CIRCLE('',#8560,8.5) ;
#3257 = CIRCLE('',#8563,8.15) ;
#3258 = CIRCLE('',#8564,8.5) ;
#3259 = CIRCLE('',#8567,8.15) ;
#3260 = CIRCLE('',#8568,8.5) ;
#3261 = CIRCLE('',#8571,8.15) ;
#3262 = CIRCLE('',#8572,8.5) ;
#3263 = CIRCLE('',#8575,8.15) ;
#3264 = CIRCLE('',#8576,8.5) ;
#3265 = CIRCLE('',#8579,8.15) ;
#3266 = CIRCLE('',#8580,8.5) ;
#3267 = CIRCLE('',#8583,8.15) ;
#3268 = CIRCLE('',#8584,8.5) ;
#3269 = CIRCLE('',#8586,8.15) ;
#3270 = CIRCLE('',#8587,8.15) ;
#3271 = CIRCLE('',#8589,8.5) ;
#3272 = CIRCLE('',#8591,8.5) ;
#3273 = CIRCLE('',#8595,1.5875) ;
#3274 = CIRCLE('',#8598,1.954) ;
#3275 = CIRCLE('',#8612,1.954) ;
#3276 = CIRCLE('',#8614,1.5555) ;
#3277 = CIRCLE('',#8628,1.954) ;
#3278 = CIRCLE('',#8630,1.954) ;
#3279 = CIRCLE('',#8631,1.5555) ;
#3280 = CIRCLE('',#8632,1.954) ;
#3281 = CIRCLE('',#8635,0.2) ;
#3282 = CIRCLE('',#8636,2.154) ;
#3283 = CIRCLE('',#8638,1.954) ;
#3284 = CIRCLE('',#8640,3.3) ;
#3285 = CIRCLE('',#8642,1.454) ;
#3286 = CIRCLE('',#8646,3.5) ;
#3287 = CIRCLE('',#8649,3.5) ;
#3288 = CIRCLE('',#8650,3.5) ;
#3289 = CIRCLE('',#8651,3.5) ;
#3290 = CIRCLE('',#8652,3.5) ;
#3291 = CIRCLE('',#8653,3.5) ;
#3292 = CIRCLE('',#8654,3.5) ;
#3293 = CIRCLE('',#8655,3.5) ;
#3294 = CIRCLE('',#8656,3.5) ;
#3295 = CIRCLE('',#8657,3.5) ;
#3296 = CIRCLE('',#8658,3.5) ;
#3297 = CIRCLE('',#8659,3.5) ;
#3298 = CIRCLE('',#8660,3.5) ;
#3299 = CIRCLE('',#8661,3.5) ;
#3300 = CIRCLE('',#8662,3.5) ;
#3301 = CIRCLE('',#8663,3.5) ;
#3302 = CIRCLE('',#8664,3.5) ;
#3303 = CIRCLE('',#8665,3.5) ;
#3304 = CIRCLE('',#8666,3.5) ;
#3305 = CIRCLE('',#8667,3.5) ;
#3306 = CIRCLE('',#8668,3.5) ;
#3307 = CIRCLE('',#8669,3.5) ;
#3308 = CIRCLE('',#8670,3.5) ;
#3309 = CIRCLE('',#8671,3.5) ;
#3310 = CIRCLE('',#8672,3.5) ;
#3311 = CIRCLE('',#8673,3.5) ;
#3312 = CIRCLE('',#8674,3.5) ;
#3313 = CIRCLE('',#8675,3.5) ;
#3314 = CIRCLE('',#8676,3.5) ;
#3315 = CIRCLE('',#8677,3.5) ;
#3316 = CIRCLE('',#8678,3.5) ;
#3317 = CIRCLE('',#8679,3.5) ;
#3318 = CIRCLE('',#8680,3.5) ;
#3319 = CIRCLE('',#8681,3.5) ;
#3320 = CIRCLE('',#8682,3.5) ;
#3321 = CIRCLE('',#8683,3.5) ;
#3322 = CIRCLE('',#8684,3.5) ;
#3323 = CIRCLE('',#8685,3.5) ;
#3324 = CIRCLE('',#8686,3.5) ;
#3325 = CIRCLE('',#8687,3.5) ;
#3326 = CIRCLE('',#8688,3.5) ;
#3327 = CIRCLE('',#8689,3.5) ;
#3328 = CIRCLE('',#8690,3.5) ;
#3329 = CIRCLE('',#8691,3.5) ;
#3330 = CIRCLE('',#8692,3.5) ;
#3331 = CIRCLE('',#8693,3.5) ;
#3332 = CIRCLE('',#8694,3.5) ;
#3333 = CIRCLE('',#8695,3.5) ;
#3334 = CIRCLE('',#8696,3.5) ;
#3335 = CIRCLE('',#8697,3.5) ;
#3336 = CIRCLE('',#8698,3.5) ;
#3337 = CIRCLE('',#8699,3.5) ;
#3338 = CIRCLE('',#8700,3.5) ;
#3339 = CIRCLE('',#8701,3.5) ;
#3340 = CIRCLE('',#8702,3.5) ;
#3341 = CIRCLE('',#8703,3.5) ;
#3342 = CIRCLE('',#8704,3.5) ;
#3343 = CIRCLE('',#8705,3.5) ;
#3344 = CIRCLE('',#8706,3.5) ;
#3345 = CIRCLE('',#8707,3.5) ;
#3346 = CIRCLE('',#8708,3.5) ;
#3347 = CIRCLE('',#8709,3.5) ;
#3348 = CIRCLE('',#8710,3.5) ;
#3349 = CIRCLE('',#8711,3.5) ;
#3350 = CIRCLE('',#8712,3.5) ;
#3351 = CIRCLE('',#8713,3.5) ;
#3352 = CIRCLE('',#8714,3.5) ;
#3353 = CIRCLE('',#8715,3.5) ;
#3354 = CIRCLE('',#8716,3.5) ;
#3355 = CIRCLE('',#8717,3.5) ;
#3356 = CIRCLE('',#8718,3.5) ;
#3357 = CIRCLE('',#8719,3.5) ;
#3358 = CIRCLE('',#8720,3.5) ;
#3359 = CIRCLE('',#8721,3.5) ;
#3360 = CIRCLE('',#8828,0.2) ;
#3361 = CIRCLE('',#8830,3.1) ;
#3362 = CIRCLE('',#8832,1.98205080756888) ;
#3363 = CIRCLE('',#8834,1.68205080756887) ;
#3364 = CIRCLE('',#8835,1.68205080756887) ;
#3365 = CIRCLE('',#8836,1.68205080756887) ;
#3366 = CIRCLE('',#8837,1.68205080756887) ;
#3367 = CIRCLE('',#8838,1.68205080756887) ;
#3368 = CIRCLE('',#8839,1.68205080756887) ;
#3369 = CIRCLE('',#8841,1.68205080756887) ;
#3370 = CIRCLE('',#8843,1.68205080756887) ;
#3371 = CIRCLE('',#8845,1.68205080756887) ;
#3372 = CIRCLE('',#8847,1.68205080756887) ;
#3373 = CIRCLE('',#8849,1.68205080756887) ;
#3374 = CIRCLE('',#8851,1.68205080756887) ;
#3375 = CIRCLE('',#8862,1.73205080756887) ;
#3376 = CIRCLE('',#8864,1.73205080756887) ;
#3377 = CIRCLE('',#8866,1.73205080756887) ;
#3378 = CIRCLE('',#8868,1.73205080756887) ;
#3379 = CIRCLE('',#8870,1.73205080756887) ;
#3380 = CIRCLE('',#8872,1.73205080756887) ;
#3381 = CIRCLE('',#8879,12.) ;
#3382 = CIRCLE('',#8880,9.) ;
#3383 = CIRCLE('',#8882,12.) ;
#3384 = CIRCLE('',#8884,9.2) ;
#3385 = CIRCLE('',#8886,8.05) ;
#3386 = CIRCLE('',#8888,8.05) ;
#3387 = CIRCLE('',#8890,8.6) ;
#3388 = CIRCLE('',#8892,8.05) ;
#3389 = CIRCLE('',#8894,8.05) ;
#3390 = CIRCLE('',#8898,0.85) ;
#3391 = CIRCLE('',#8899,0.85) ;
#3392 = CIRCLE('',#8904,10.2) ;
#3393 = CIRCLE('',#8905,12.55) ;
#3394 = CIRCLE('',#8906,0.85) ;
#3395 = CIRCLE('',#8908,0.85) ;
#3396 = CIRCLE('',#8912,10.2) ;
#3397 = CIRCLE('',#8915,12.55) ;
#3398 = VERTEX_POINT('',#10955) ;
#3399 = VERTEX_POINT('',#10957) ;
#3400 = VERTEX_POINT('',#10961) ;
#3401 = VERTEX_POINT('',#10963) ;
#3402 = VERTEX_POINT('',#10967) ;
#3403 = VERTEX_POINT('',#10970) ;
#3404 = VERTEX_POINT('',#10973) ;
#3405 = VERTEX_POINT('',#10975) ;
#3406 = VERTEX_POINT('',#10979) ;
#3407 = VERTEX_POINT('',#10981) ;
#3408 = VERTEX_POINT('',#10985) ;
#3409 = VERTEX_POINT('',#10988) ;
#3410 = VERTEX_POINT('',#10991) ;
#3411 = VERTEX_POINT('',#10992) ;
#3412 = VERTEX_POINT('',#10994) ;
#3413 = VERTEX_POINT('',#10998) ;
#3414 = VERTEX_POINT('',#11000) ;
#3415 = VERTEX_POINT('',#11004) ;
#3416 = VERTEX_POINT('',#11008) ;
#3417 = VERTEX_POINT('',#11009) ;
#3418 = VERTEX_POINT('',#11013) ;
#3419 = VERTEX_POINT('',#11015) ;
#3420 = VERTEX_POINT('',#11021) ;
#3421 = VERTEX_POINT('',#11022) ;
#3422 = VERTEX_POINT('',#11029) ;
#3423 = VERTEX_POINT('',#11031) ;
#3424 = VERTEX_POINT('',#11039) ;
#3425 = VERTEX_POINT('',#11041) ;
#3426 = VERTEX_POINT('',#11049) ;
#3427 = VERTEX_POINT('',#11051) ;
#3428 = VERTEX_POINT('',#11060) ;
#3429 = VERTEX_POINT('',#11061) ;
#3430 = VERTEX_POINT('',#11068) ;
#3431 = VERTEX_POINT('',#11070) ;
#3432 = VERTEX_POINT('',#11078) ;
#3433 = VERTEX_POINT('',#11080) ;
#3434 = VERTEX_POINT('',#11088) ;
#3435 = VERTEX_POINT('',#11090) ;
#3436 = VERTEX_POINT('',#11099) ;
#3437 = VERTEX_POINT('',#11100) ;
#3438 = VERTEX_POINT('',#11108) ;
#3439 = VERTEX_POINT('',#11110) ;
#3440 = VERTEX_POINT('',#11118) ;
#3441 = VERTEX_POINT('',#11120) ;
#3442 = VERTEX_POINT('',#11127) ;
#3443 = VERTEX_POINT('',#11129) ;
#3444 = VERTEX_POINT('',#11138) ;
#3445 = VERTEX_POINT('',#11139) ;
#3446 = VERTEX_POINT('',#11147) ;
#3447 = VERTEX_POINT('',#11149) ;
#3448 = VERTEX_POINT('',#11157) ;
#3449 = VERTEX_POINT('',#11159) ;
#3450 = VERTEX_POINT('',#11166) ;
#3451 = VERTEX_POINT('',#11168) ;
#3452 = VERTEX_POINT('',#11205) ;
#3453 = VERTEX_POINT('',#11208) ;
#3454 = VERTEX_POINT('',#11214) ;
#3455 = VERTEX_POINT('',#11217) ;
#3456 = VERTEX_POINT('',#11230) ;
#3457 = VERTEX_POINT('',#11231) ;
#3458 = VERTEX_POINT('',#11242) ;
#3459 = VERTEX_POINT('',#11244) ;
#3460 = VERTEX_POINT('',#11255) ;
#3461 = VERTEX_POINT('',#11266) ;
#3462 = VERTEX_POINT('',#11277) ;
#3463 = VERTEX_POINT('',#11288) ;
#3464 = VERTEX_POINT('',#11299) ;
#3465 = VERTEX_POINT('',#11310) ;
#3466 = VERTEX_POINT('',#11321) ;
#3467 = VERTEX_POINT('',#11322) ;
#3468 = VERTEX_POINT('',#11333) ;
#3469 = VERTEX_POINT('',#11335) ;
#3470 = VERTEX_POINT('',#11346) ;
#3471 = VERTEX_POINT('',#11354) ;
#3472 = VERTEX_POINT('',#11365) ;
#3473 = VERTEX_POINT('',#11373) ;
#3474 = VERTEX_POINT('',#11384) ;
#3475 = VERTEX_POINT('',#11392) ;
#3476 = VERTEX_POINT('',#11403) ;
#3477 = VERTEX_POINT('',#11411) ;
#3478 = VERTEX_POINT('',#11422) ;
#3479 = VERTEX_POINT('',#11433) ;
#3480 = VERTEX_POINT('',#11444) ;
#3481 = VERTEX_POINT('',#11451) ;
#3482 = VERTEX_POINT('',#11462) ;
#3483 = VERTEX_POINT('',#11471) ;
#3484 = VERTEX_POINT('',#11482) ;
#3485 = VERTEX_POINT('',#11493) ;
#3486 = VERTEX_POINT('',#11504) ;
#3487 = VERTEX_POINT('',#11512) ;
#3488 = VERTEX_POINT('',#11523) ;
#3489 = VERTEX_POINT('',#11531) ;
#3490 = VERTEX_POINT('',#11542) ;
#3491 = VERTEX_POINT('',#11550) ;
#3492 = VERTEX_POINT('',#11561) ;
#3493 = VERTEX_POINT('',#11569) ;
#3494 = VERTEX_POINT('',#11596) ;
#3495 = VERTEX_POINT('',#11604) ;
#3496 = VERTEX_POINT('',#11615) ;
#3497 = VERTEX_POINT('',#11623) ;
#3498 = VERTEX_POINT('',#11634) ;
#3499 = VERTEX_POINT('',#11642) ;
#3500 = VERTEX_POINT('',#11653) ;
#3501 = VERTEX_POINT('',#11667) ;
#3502 = VERTEX_POINT('',#11678) ;
#3503 = VERTEX_POINT('',#11686) ;
#3504 = VERTEX_POINT('',#11697) ;
#3505 = VERTEX_POINT('',#11705) ;
#3506 = VERTEX_POINT('',#11716) ;
#3507 = VERTEX_POINT('',#11727) ;
#3508 = VERTEX_POINT('',#11738) ;
#3509 = VERTEX_POINT('',#11752) ;
#3510 = VERTEX_POINT('',#11758) ;
#3511 = VERTEX_POINT('',#11760) ;
#3512 = VERTEX_POINT('',#11786) ;
#3513 = VERTEX_POINT('',#11787) ;
#3514 = VERTEX_POINT('',#11795) ;
#3515 = VERTEX_POINT('',#11797) ;
#3516 = VERTEX_POINT('',#11803) ;
#3517 = VERTEX_POINT('',#11805) ;
#3518 = VERTEX_POINT('',#11814) ;
#3519 = VERTEX_POINT('',#11822) ;
#3520 = VERTEX_POINT('',#11833) ;
#3521 = VERTEX_POINT('',#11841) ;
#3522 = VERTEX_POINT('',#11847) ;
#3523 = VERTEX_POINT('',#11849) ;
#3524 = VERTEX_POINT('',#11858) ;
#3525 = VERTEX_POINT('',#11866) ;
#3526 = VERTEX_POINT('',#11872) ;
#3527 = VERTEX_POINT('',#11874) ;
#3528 = VERTEX_POINT('',#11878) ;
#3529 = VERTEX_POINT('',#11880) ;
#3530 = VERTEX_POINT('',#11888) ;
#3531 = VERTEX_POINT('',#11890) ;
#3532 = VERTEX_POINT('',#11893) ;
#3533 = VERTEX_POINT('',#11894) ;
#3534 = VERTEX_POINT('',#11896) ;
#3535 = VERTEX_POINT('',#11898) ;
#3536 = VERTEX_POINT('',#11900) ;
#3537 = VERTEX_POINT('',#11902) ;
#3538 = VERTEX_POINT('',#11904) ;
#3539 = VERTEX_POINT('',#11930) ;
#3540 = VERTEX_POINT('',#11956) ;
#3541 = VERTEX_POINT('',#11958) ;
#3542 = VERTEX_POINT('',#11960) ;
#3543 = VERTEX_POINT('',#11962) ;
#3544 = VERTEX_POINT('',#11964) ;
#3545 = VERTEX_POINT('',#11966) ;
#3546 = VERTEX_POINT('',#11968) ;
#3547 = VERTEX_POINT('',#11971) ;
#3548 = VERTEX_POINT('',#11972) ;
#3549 = VERTEX_POINT('',#11980) ;
#3550 = VERTEX_POINT('',#11988) ;
#3551 = VERTEX_POINT('',#11990) ;
#3552 = VERTEX_POINT('',#11998) ;
#3553 = VERTEX_POINT('',#12006) ;
#3554 = VERTEX_POINT('',#12014) ;
#3555 = VERTEX_POINT('',#12022) ;
#3556 = VERTEX_POINT('',#12030) ;
#3557 = VERTEX_POINT('',#12038) ;
#3558 = VERTEX_POINT('',#12046) ;
#3559 = VERTEX_POINT('',#12057) ;
#3560 = VERTEX_POINT('',#12077) ;
#3561 = VERTEX_POINT('',#12091) ;
#3562 = VERTEX_POINT('',#12099) ;
#3563 = VERTEX_POINT('',#12107) ;
#3564 = VERTEX_POINT('',#12115) ;
#3565 = VERTEX_POINT('',#12123) ;
#3566 = VERTEX_POINT('',#12131) ;
#3567 = VERTEX_POINT('',#12139) ;
#3568 = VERTEX_POINT('',#12147) ;
#3569 = VERTEX_POINT('',#12155) ;
#3570 = VERTEX_POINT('',#12157) ;
#3571 = VERTEX_POINT('',#12168) ;
#3572 = VERTEX_POINT('',#12179) ;
#3573 = VERTEX_POINT('',#12193) ;
#3574 = VERTEX_POINT('',#12204) ;
#3575 = VERTEX_POINT('',#12215) ;
#3576 = VERTEX_POINT('',#12232) ;
#3577 = VERTEX_POINT('',#12252) ;
#3578 = VERTEX_POINT('',#12260) ;
#3579 = VERTEX_POINT('',#12268) ;
#3580 = VERTEX_POINT('',#12276) ;
#3581 = VERTEX_POINT('',#12284) ;
#3582 = VERTEX_POINT('',#12299) ;
#3583 = VERTEX_POINT('',#12300) ;
#3584 = VERTEX_POINT('',#12317) ;
#3585 = VERTEX_POINT('',#12319) ;
#3586 = VERTEX_POINT('',#12321) ;
#3587 = VERTEX_POINT('',#12323) ;
#3588 = VERTEX_POINT('',#12337) ;
#3589 = VERTEX_POINT('',#12345) ;
#3590 = VERTEX_POINT('',#12356) ;
#3591 = VERTEX_POINT('',#12364) ;
#3592 = VERTEX_POINT('',#12372) ;
#3593 = VERTEX_POINT('',#12386) ;
#3594 = VERTEX_POINT('',#12388) ;
#3595 = VERTEX_POINT('',#12390) ;
#3596 = VERTEX_POINT('',#12392) ;
#3597 = VERTEX_POINT('',#12409) ;
#3598 = VERTEX_POINT('',#12417) ;
#3599 = VERTEX_POINT('',#12438) ;
#3600 = VERTEX_POINT('',#12439) ;
#3601 = VERTEX_POINT('',#12441) ;
#3602 = VERTEX_POINT('',#12443) ;
#3603 = VERTEX_POINT('',#12445) ;
#3604 = VERTEX_POINT('',#12447) ;
#3605 = VERTEX_POINT('',#12449) ;
#3606 = VERTEX_POINT('',#12475) ;
#3607 = VERTEX_POINT('',#12501) ;
#3608 = VERTEX_POINT('',#12503) ;
#3609 = VERTEX_POINT('',#12505) ;
#3610 = VERTEX_POINT('',#12507) ;
#3611 = VERTEX_POINT('',#12509) ;
#3612 = VERTEX_POINT('',#12511) ;
#3613 = VERTEX_POINT('',#12513) ;
#3614 = VERTEX_POINT('',#12516) ;
#3615 = VERTEX_POINT('',#12517) ;
#3616 = VERTEX_POINT('',#12519) ;
#3617 = VERTEX_POINT('',#12521) ;
#3618 = VERTEX_POINT('',#12524) ;
#3619 = VERTEX_POINT('',#12525) ;
#3620 = VERTEX_POINT('',#12527) ;
#3621 = VERTEX_POINT('',#12529) ;
#3622 = VERTEX_POINT('',#12533) ;
#3623 = VERTEX_POINT('',#12535) ;
#3624 = VERTEX_POINT('',#12539) ;
#3625 = VERTEX_POINT('',#12543) ;
#3626 = VERTEX_POINT('',#12550) ;
#3627 = VERTEX_POINT('',#12552) ;
#3628 = VERTEX_POINT('',#12556) ;
#3629 = VERTEX_POINT('',#12560) ;
#3630 = VERTEX_POINT('',#12567) ;
#3631 = VERTEX_POINT('',#12569) ;
#3632 = VERTEX_POINT('',#12573) ;
#3633 = VERTEX_POINT('',#12577) ;
#3634 = VERTEX_POINT('',#12581) ;
#3635 = VERTEX_POINT('',#12585) ;
#3636 = VERTEX_POINT('',#12589) ;
#3637 = VERTEX_POINT('',#12593) ;
#3638 = VERTEX_POINT('',#12597) ;
#3639 = VERTEX_POINT('',#12601) ;
#3640 = VERTEX_POINT('',#12610) ;
#3641 = VERTEX_POINT('',#12621) ;
#3642 = VERTEX_POINT('',#12627) ;
#3643 = VERTEX_POINT('',#12631) ;
#3644 = VERTEX_POINT('',#12635) ;
#3645 = VERTEX_POINT('',#12647) ;
#3646 = VERTEX_POINT('',#12649) ;
#3647 = VERTEX_POINT('',#12655) ;
#3648 = VERTEX_POINT('',#12659) ;
#3649 = VERTEX_POINT('',#12663) ;
#3650 = VERTEX_POINT('',#12672) ;
#3651 = VERTEX_POINT('',#12683) ;
#3652 = VERTEX_POINT('',#12694) ;
#3653 = VERTEX_POINT('',#12705) ;
#3654 = VERTEX_POINT('',#12716) ;
#3655 = VERTEX_POINT('',#12727) ;
#3656 = VERTEX_POINT('',#12738) ;
#3657 = VERTEX_POINT('',#12749) ;
#3658 = VERTEX_POINT('',#12760) ;
#3659 = VERTEX_POINT('',#12771) ;
#3660 = VERTEX_POINT('',#12777) ;
#3661 = VERTEX_POINT('',#12781) ;
#3662 = VERTEX_POINT('',#12793) ;
#3663 = VERTEX_POINT('',#12795) ;
#3664 = VERTEX_POINT('',#12806) ;
#3665 = VERTEX_POINT('',#12817) ;
#3666 = VERTEX_POINT('',#12823) ;
#3667 = VERTEX_POINT('',#12832) ;
#3668 = VERTEX_POINT('',#12843) ;
#3669 = VERTEX_POINT('',#12854) ;
#3670 = VERTEX_POINT('',#12865) ;
#3671 = VERTEX_POINT('',#12876) ;
#3672 = VERTEX_POINT('',#12887) ;
#3673 = VERTEX_POINT('',#12898) ;
#3674 = VERTEX_POINT('',#12909) ;
#3675 = VERTEX_POINT('',#12920) ;
#3676 = VERTEX_POINT('',#12931) ;
#3677 = VERTEX_POINT('',#12942) ;
#3678 = VERTEX_POINT('',#12953) ;
#3679 = VERTEX_POINT('',#12964) ;
#3680 = VERTEX_POINT('',#12975) ;
#3681 = VERTEX_POINT('',#12986) ;
#3682 = VERTEX_POINT('',#12997) ;
#3683 = VERTEX_POINT('',#13008) ;
#3684 = VERTEX_POINT('',#13019) ;
#3685 = VERTEX_POINT('',#13030) ;
#3686 = VERTEX_POINT('',#13041) ;
#3687 = VERTEX_POINT('',#13052) ;
#3688 = VERTEX_POINT('',#13063) ;
#3689 = VERTEX_POINT('',#13074) ;
#3690 = VERTEX_POINT('',#13085) ;
#3691 = VERTEX_POINT('',#13096) ;
#3692 = VERTEX_POINT('',#13107) ;
#3693 = VERTEX_POINT('',#13118) ;
#3694 = VERTEX_POINT('',#13129) ;
#3695 = VERTEX_POINT('',#13140) ;
#3696 = VERTEX_POINT('',#13146) ;
#3697 = VERTEX_POINT('',#13160) ;
#3698 = VERTEX_POINT('',#13162) ;
#3699 = VERTEX_POINT('',#13166) ;
#3700 = VERTEX_POINT('',#13170) ;
#3701 = VERTEX_POINT('',#13174) ;
#3702 = VERTEX_POINT('',#13178) ;
#3703 = VERTEX_POINT('',#13182) ;
#3704 = VERTEX_POINT('',#13186) ;
#3705 = VERTEX_POINT('',#13190) ;
#3706 = VERTEX_POINT('',#13194) ;
#3707 = VERTEX_POINT('',#13203) ;
#3708 = VERTEX_POINT('',#13214) ;
#3709 = VERTEX_POINT('',#13220) ;
#3710 = VERTEX_POINT('',#13224) ;
#3711 = VERTEX_POINT('',#13228) ;
#3712 = VERTEX_POINT('',#13235) ;
#3713 = VERTEX_POINT('',#13237) ;
#3714 = VERTEX_POINT('',#13241) ;
#3715 = VERTEX_POINT('',#13246) ;
#3716 = VERTEX_POINT('',#13247) ;
#3717 = VERTEX_POINT('',#13249) ;
#3718 = VERTEX_POINT('',#13251) ;
#3719 = VERTEX_POINT('',#13253) ;
#3720 = VERTEX_POINT('',#13293) ;
#3721 = VERTEX_POINT('',#13295) ;
#3722 = VERTEX_POINT('',#13302) ;
#3723 = VERTEX_POINT('',#13304) ;
#3724 = VERTEX_POINT('',#13311) ;
#3725 = VERTEX_POINT('',#13313) ;
#3726 = VERTEX_POINT('',#13320) ;
#3727 = VERTEX_POINT('',#13322) ;
#3728 = VERTEX_POINT('',#13324) ;
#3729 = VERTEX_POINT('',#13329) ;
#3730 = VERTEX_POINT('',#13333) ;
#3731 = VERTEX_POINT('',#13335) ;
#3732 = VERTEX_POINT('',#13337) ;
#3733 = VERTEX_POINT('',#13372) ;
#3734 = VERTEX_POINT('',#13376) ;
#3735 = VERTEX_POINT('',#13378) ;
#3736 = VERTEX_POINT('',#13380) ;
#3737 = VERTEX_POINT('',#13415) ;
#3738 = VERTEX_POINT('',#13419) ;
#3739 = VERTEX_POINT('',#13421) ;
#3740 = VERTEX_POINT('',#13423) ;
#3741 = VERTEX_POINT('',#13458) ;
#3742 = VERTEX_POINT('',#13462) ;
#3743 = VERTEX_POINT('',#13465) ;
#3744 = VERTEX_POINT('',#13468) ;
#3745 = VERTEX_POINT('',#13471) ;
#3746 = VERTEX_POINT('',#13474) ;
#3747 = VERTEX_POINT('',#13478) ;
#3748 = VERTEX_POINT('',#13482) ;
#3749 = VERTEX_POINT('',#13486) ;
#3750 = VERTEX_POINT('',#13490) ;
#3751 = VERTEX_POINT('',#13491) ;
#3752 = VERTEX_POINT('',#13493) ;
#3753 = VERTEX_POINT('',#13495) ;
#3754 = VERTEX_POINT('',#13499) ;
#3755 = VERTEX_POINT('',#13500) ;
#3756 = VERTEX_POINT('',#13502) ;
#3757 = VERTEX_POINT('',#13504) ;
#3758 = VERTEX_POINT('',#13508) ;
#3759 = VERTEX_POINT('',#13509) ;
#3760 = VERTEX_POINT('',#13511) ;
#3761 = VERTEX_POINT('',#13513) ;
#3762 = VERTEX_POINT('',#13517) ;
#3763 = VERTEX_POINT('',#13518) ;
#3764 = VERTEX_POINT('',#13520) ;
#3765 = VERTEX_POINT('',#13522) ;
#3766 = VERTEX_POINT('',#13526) ;
#3767 = VERTEX_POINT('',#13541) ;
#3768 = VERTEX_POINT('',#13546) ;
#3769 = VERTEX_POINT('',#13548) ;
#3770 = VERTEX_POINT('',#13551) ;
#3771 = VERTEX_POINT('',#13555) ;
#3772 = VERTEX_POINT('',#13558) ;
#3773 = VERTEX_POINT('',#13562) ;
#3774 = VERTEX_POINT('',#13564) ;
#3775 = VERTEX_POINT('',#13567) ;
#3776 = VERTEX_POINT('',#13571) ;
#3777 = VERTEX_POINT('',#13574) ;
#3778 = VERTEX_POINT('',#13579) ;
#3779 = VERTEX_POINT('',#13583) ;
#3780 = VERTEX_POINT('',#13586) ;
#3781 = VERTEX_POINT('',#13590) ;
#3782 = VERTEX_POINT('',#13596) ;
#3783 = VERTEX_POINT('',#13604) ;
#3784 = VERTEX_POINT('',#13605) ;
#3785 = VERTEX_POINT('',#13607) ;
#3786 = VERTEX_POINT('',#13609) ;
#3787 = VERTEX_POINT('',#13613) ;
#3788 = VERTEX_POINT('',#13615) ;
#3789 = VERTEX_POINT('',#13619) ;
#3790 = VERTEX_POINT('',#13621) ;
#3791 = VERTEX_POINT('',#13628) ;
#3792 = VERTEX_POINT('',#13629) ;
#3793 = VERTEX_POINT('',#13631) ;
#3794 = VERTEX_POINT('',#13633) ;
#3795 = VERTEX_POINT('',#13637) ;
#3796 = VERTEX_POINT('',#13639) ;
#3797 = VERTEX_POINT('',#13643) ;
#3798 = VERTEX_POINT('',#13645) ;
#3799 = VERTEX_POINT('',#13652) ;
#3800 = VERTEX_POINT('',#13653) ;
#3801 = VERTEX_POINT('',#13655) ;
#3802 = VERTEX_POINT('',#13657) ;
#3803 = VERTEX_POINT('',#13661) ;
#3804 = VERTEX_POINT('',#13663) ;
#3805 = VERTEX_POINT('',#13667) ;
#3806 = VERTEX_POINT('',#13669) ;
#3807 = VERTEX_POINT('',#13676) ;
#3808 = VERTEX_POINT('',#13677) ;
#3809 = VERTEX_POINT('',#13679) ;
#3810 = VERTEX_POINT('',#13681) ;
#3811 = VERTEX_POINT('',#13685) ;
#3812 = VERTEX_POINT('',#13687) ;
#3813 = VERTEX_POINT('',#13691) ;
#3814 = VERTEX_POINT('',#13693) ;
#3815 = VERTEX_POINT('',#13700) ;
#3816 = VERTEX_POINT('',#13702) ;
#3817 = VERTEX_POINT('',#13706) ;
#3818 = VERTEX_POINT('',#13709) ;
#3819 = VERTEX_POINT('',#13715) ;
#3820 = VERTEX_POINT('',#13716) ;
#3821 = VERTEX_POINT('',#13720) ;
#3822 = VERTEX_POINT('',#13721) ;
#3823 = VERTEX_POINT('',#13723) ;
#3824 = VERTEX_POINT('',#13734) ;
#3825 = VERTEX_POINT('',#13744) ;
#3826 = VERTEX_POINT('',#13745) ;
#3827 = VERTEX_POINT('',#13792) ;
#3828 = VERTEX_POINT('',#13793) ;
#3829 = VERTEX_POINT('',#13840) ;
#3830 = VERTEX_POINT('',#13841) ;
#3831 = VERTEX_POINT('',#13894) ;
#3832 = VERTEX_POINT('',#13895) ;
#3833 = VERTEX_POINT('',#13942) ;
#3834 = VERTEX_POINT('',#13943) ;
#3835 = VERTEX_POINT('',#13990) ;
#3836 = VERTEX_POINT('',#13991) ;
#3837 = VERTEX_POINT('',#14044) ;
#3838 = VERTEX_POINT('',#14045) ;
#3839 = VERTEX_POINT('',#14092) ;
#3840 = VERTEX_POINT('',#14093) ;
#3841 = VERTEX_POINT('',#14140) ;
#3842 = VERTEX_POINT('',#14141) ;
#3843 = VERTEX_POINT('',#14188) ;
#3844 = VERTEX_POINT('',#14189) ;
#3845 = VERTEX_POINT('',#14242) ;
#3846 = VERTEX_POINT('',#14243) ;
#3847 = VERTEX_POINT('',#14290) ;
#3848 = VERTEX_POINT('',#14291) ;
#3849 = VERTEX_POINT('',#14338) ;
#3850 = VERTEX_POINT('',#14339) ;
#3851 = VERTEX_POINT('',#14341) ;
#3852 = VERTEX_POINT('',#14391) ;
#3853 = VERTEX_POINT('',#14392) ;
#3854 = VERTEX_POINT('',#14394) ;
#3855 = VERTEX_POINT('',#14403) ;
#3856 = VERTEX_POINT('',#14412) ;
#3857 = VERTEX_POINT('',#14413) ;
#3858 = VERTEX_POINT('',#14437) ;
#3859 = VERTEX_POINT('',#14438) ;
#3860 = VERTEX_POINT('',#14461) ;
#3861 = VERTEX_POINT('',#14462) ;
#3862 = VERTEX_POINT('',#14486) ;
#3863 = VERTEX_POINT('',#14487) ;
#3864 = VERTEX_POINT('',#14511) ;
#3865 = VERTEX_POINT('',#14512) ;
#3866 = VERTEX_POINT('',#14535) ;
#3867 = VERTEX_POINT('',#14536) ;
#3868 = VERTEX_POINT('',#14559) ;
#3869 = VERTEX_POINT('',#14560) ;
#3870 = VERTEX_POINT('',#14584) ;
#3871 = VERTEX_POINT('',#14585) ;
#3872 = VERTEX_POINT('',#14609) ;
#3873 = VERTEX_POINT('',#14610) ;
#3874 = VERTEX_POINT('',#14633) ;
#3875 = VERTEX_POINT('',#14634) ;
#3876 = VERTEX_POINT('',#14658) ;
#3877 = VERTEX_POINT('',#14659) ;
#3878 = VERTEX_POINT('',#14683) ;
#3879 = VERTEX_POINT('',#14684) ;
#3880 = VERTEX_POINT('',#14795) ;
#3881 = VERTEX_POINT('',#15245) ;
#3882 = VERTEX_POINT('',#15344) ;
#3883 = VERTEX_POINT('',#15346) ;
#3884 = VERTEX_POINT('',#15803) ;
#3885 = VERTEX_POINT('',#15809) ;
#3886 = VERTEX_POINT('',#15812) ;
#3887 = VERTEX_POINT('',#15817) ;
#3888 = VERTEX_POINT('',#15818) ;
#3889 = VERTEX_POINT('',#15822) ;
#3890 = VERTEX_POINT('',#15824) ;
#3891 = VERTEX_POINT('',#15828) ;
#3892 = VERTEX_POINT('',#15832) ;
#3893 = VERTEX_POINT('',#15838) ;
#3894 = VERTEX_POINT('',#15840) ;
#3895 = VERTEX_POINT('',#15842) ;
#3896 = VERTEX_POINT('',#15844) ;
#3897 = VERTEX_POINT('',#15846) ;
#3898 = VERTEX_POINT('',#15848) ;
#3899 = VERTEX_POINT('',#15850) ;
#3900 = VERTEX_POINT('',#15852) ;
#3901 = VERTEX_POINT('',#15854) ;
#3902 = VERTEX_POINT('',#15856) ;
#3903 = VERTEX_POINT('',#15858) ;
#3904 = VERTEX_POINT('',#15860) ;
#3905 = VERTEX_POINT('',#15862) ;
#3906 = VERTEX_POINT('',#15864) ;
#3907 = VERTEX_POINT('',#15866) ;
#3908 = VERTEX_POINT('',#15868) ;
#3909 = VERTEX_POINT('',#15870) ;
#3910 = VERTEX_POINT('',#15872) ;
#3911 = VERTEX_POINT('',#15874) ;
#3912 = VERTEX_POINT('',#15876) ;
#3913 = VERTEX_POINT('',#15878) ;
#3914 = VERTEX_POINT('',#15880) ;
#3915 = VERTEX_POINT('',#15882) ;
#3916 = VERTEX_POINT('',#15884) ;
#3917 = VERTEX_POINT('',#15886) ;
#3918 = VERTEX_POINT('',#15888) ;
#3919 = VERTEX_POINT('',#15890) ;
#3920 = VERTEX_POINT('',#15892) ;
#3921 = VERTEX_POINT('',#15894) ;
#3922 = VERTEX_POINT('',#15896) ;
#3923 = VERTEX_POINT('',#15898) ;
#3924 = VERTEX_POINT('',#15900) ;
#3925 = VERTEX_POINT('',#15902) ;
#3926 = VERTEX_POINT('',#15904) ;
#3927 = VERTEX_POINT('',#15906) ;
#3928 = VERTEX_POINT('',#15908) ;
#3929 = VERTEX_POINT('',#15910) ;
#3930 = VERTEX_POINT('',#15912) ;
#3931 = VERTEX_POINT('',#15914) ;
#3932 = VERTEX_POINT('',#15916) ;
#3933 = VERTEX_POINT('',#15918) ;
#3934 = VERTEX_POINT('',#15920) ;
#3935 = VERTEX_POINT('',#15922) ;
#3936 = VERTEX_POINT('',#15924) ;
#3937 = VERTEX_POINT('',#15926) ;
#3938 = VERTEX_POINT('',#15928) ;
#3939 = VERTEX_POINT('',#15930) ;
#3940 = VERTEX_POINT('',#15932) ;
#3941 = VERTEX_POINT('',#15934) ;
#3942 = VERTEX_POINT('',#15936) ;
#3943 = VERTEX_POINT('',#15938) ;
#3944 = VERTEX_POINT('',#15940) ;
#3945 = VERTEX_POINT('',#15942) ;
#3946 = VERTEX_POINT('',#15944) ;
#3947 = VERTEX_POINT('',#15946) ;
#3948 = VERTEX_POINT('',#15948) ;
#3949 = VERTEX_POINT('',#15950) ;
#3950 = VERTEX_POINT('',#15952) ;
#3951 = VERTEX_POINT('',#15954) ;
#3952 = VERTEX_POINT('',#15956) ;
#3953 = VERTEX_POINT('',#15958) ;
#3954 = VERTEX_POINT('',#15960) ;
#3955 = VERTEX_POINT('',#15962) ;
#3956 = VERTEX_POINT('',#15964) ;
#3957 = VERTEX_POINT('',#15966) ;
#3958 = VERTEX_POINT('',#15968) ;
#3959 = VERTEX_POINT('',#15970) ;
#3960 = VERTEX_POINT('',#15972) ;
#3961 = VERTEX_POINT('',#15974) ;
#3962 = VERTEX_POINT('',#15976) ;
#3963 = VERTEX_POINT('',#15978) ;
#3964 = VERTEX_POINT('',#15980) ;
#3965 = VERTEX_POINT('',#15982) ;
#3966 = VERTEX_POINT('',#15984) ;
#3967 = VERTEX_POINT('',#15986) ;
#3968 = VERTEX_POINT('',#15988) ;
#3969 = VERTEX_POINT('',#15990) ;
#3970 = VERTEX_POINT('',#15992) ;
#3971 = VERTEX_POINT('',#15994) ;
#3972 = VERTEX_POINT('',#15996) ;
#3973 = VERTEX_POINT('',#15998) ;
#3974 = VERTEX_POINT('',#16000) ;
#3975 = VERTEX_POINT('',#16002) ;
#3976 = VERTEX_POINT('',#16004) ;
#3977 = VERTEX_POINT('',#16006) ;
#3978 = VERTEX_POINT('',#16008) ;
#3979 = VERTEX_POINT('',#16010) ;
#3980 = VERTEX_POINT('',#16012) ;
#3981 = VERTEX_POINT('',#16014) ;
#3982 = VERTEX_POINT('',#16016) ;
#3983 = VERTEX_POINT('',#16018) ;
#3984 = VERTEX_POINT('',#16020) ;
#3985 = VERTEX_POINT('',#16022) ;
#3986 = VERTEX_POINT('',#16024) ;
#3987 = VERTEX_POINT('',#16026) ;
#3988 = VERTEX_POINT('',#16028) ;
#3989 = VERTEX_POINT('',#16030) ;
#3990 = VERTEX_POINT('',#16032) ;
#3991 = VERTEX_POINT('',#16034) ;
#3992 = VERTEX_POINT('',#16036) ;
#3993 = VERTEX_POINT('',#16038) ;
#3994 = VERTEX_POINT('',#16040) ;
#3995 = VERTEX_POINT('',#16042) ;
#3996 = VERTEX_POINT('',#16044) ;
#3997 = VERTEX_POINT('',#16046) ;
#3998 = VERTEX_POINT('',#16048) ;
#3999 = VERTEX_POINT('',#16050) ;
#4000 = VERTEX_POINT('',#16052) ;
#4001 = VERTEX_POINT('',#16054) ;
#4002 = VERTEX_POINT('',#16056) ;
#4003 = VERTEX_POINT('',#16058) ;
#4004 = VERTEX_POINT('',#16060) ;
#4005 = VERTEX_POINT('',#16063) ;
#4006 = VERTEX_POINT('',#16065) ;
#4007 = VERTEX_POINT('',#16067) ;
#4008 = VERTEX_POINT('',#16069) ;
#4009 = VERTEX_POINT('',#16071) ;
#4010 = VERTEX_POINT('',#16073) ;
#4011 = VERTEX_POINT('',#16075) ;
#4012 = VERTEX_POINT('',#16077) ;
#4013 = VERTEX_POINT('',#16079) ;
#4014 = VERTEX_POINT('',#16081) ;
#4015 = VERTEX_POINT('',#16083) ;
#4016 = VERTEX_POINT('',#16085) ;
#4017 = VERTEX_POINT('',#16087) ;
#4018 = VERTEX_POINT('',#16089) ;
#4019 = VERTEX_POINT('',#16091) ;
#4020 = VERTEX_POINT('',#16093) ;
#4021 = VERTEX_POINT('',#16095) ;
#4022 = VERTEX_POINT('',#16097) ;
#4023 = VERTEX_POINT('',#16099) ;
#4024 = VERTEX_POINT('',#16101) ;
#4025 = VERTEX_POINT('',#16103) ;
#4026 = VERTEX_POINT('',#16105) ;
#4027 = VERTEX_POINT('',#16107) ;
#4028 = VERTEX_POINT('',#16109) ;
#4029 = VERTEX_POINT('',#16111) ;
#4030 = VERTEX_POINT('',#16113) ;
#4031 = VERTEX_POINT('',#16115) ;
#4032 = VERTEX_POINT('',#16117) ;
#4033 = VERTEX_POINT('',#16119) ;
#4034 = VERTEX_POINT('',#16121) ;
#4035 = VERTEX_POINT('',#16125) ;
#4036 = VERTEX_POINT('',#16129) ;
#4037 = VERTEX_POINT('',#16139) ;
#4038 = VERTEX_POINT('',#16143) ;
#4039 = VERTEX_POINT('',#16153) ;
#4040 = VERTEX_POINT('',#16157) ;
#4041 = VERTEX_POINT('',#16167) ;
#4042 = VERTEX_POINT('',#16171) ;
#4043 = VERTEX_POINT('',#16181) ;
#4044 = VERTEX_POINT('',#16185) ;
#4045 = VERTEX_POINT('',#16195) ;
#4046 = VERTEX_POINT('',#16199) ;
#4047 = VERTEX_POINT('',#16209) ;
#4048 = VERTEX_POINT('',#16213) ;
#4049 = VERTEX_POINT('',#16223) ;
#4050 = VERTEX_POINT('',#16227) ;
#4051 = VERTEX_POINT('',#16237) ;
#4052 = VERTEX_POINT('',#16241) ;
#4053 = VERTEX_POINT('',#16251) ;
#4054 = VERTEX_POINT('',#16255) ;
#4055 = VERTEX_POINT('',#16265) ;
#4056 = VERTEX_POINT('',#16269) ;
#4057 = VERTEX_POINT('',#16279) ;
#4058 = VERTEX_POINT('',#16283) ;
#4059 = VERTEX_POINT('',#16293) ;
#4060 = VERTEX_POINT('',#16297) ;
#4061 = VERTEX_POINT('',#16307) ;
#4062 = VERTEX_POINT('',#16311) ;
#4063 = VERTEX_POINT('',#16321) ;
#4064 = VERTEX_POINT('',#16325) ;
#4065 = VERTEX_POINT('',#16335) ;
#4066 = VERTEX_POINT('',#16339) ;
#4067 = VERTEX_POINT('',#16349) ;
#4068 = VERTEX_POINT('',#16353) ;
#4069 = VERTEX_POINT('',#16363) ;
#4070 = VERTEX_POINT('',#16367) ;
#4071 = VERTEX_POINT('',#16377) ;
#4072 = VERTEX_POINT('',#16381) ;
#4073 = VERTEX_POINT('',#16391) ;
#4074 = VERTEX_POINT('',#16395) ;
#4075 = VERTEX_POINT('',#16405) ;
#4076 = VERTEX_POINT('',#16409) ;
#4077 = VERTEX_POINT('',#16419) ;
#4078 = VERTEX_POINT('',#16423) ;
#4079 = VERTEX_POINT('',#16433) ;
#4080 = VERTEX_POINT('',#16437) ;
#4081 = VERTEX_POINT('',#16447) ;
#4082 = VERTEX_POINT('',#16451) ;
#4083 = VERTEX_POINT('',#16461) ;
#4084 = VERTEX_POINT('',#16465) ;
#4085 = VERTEX_POINT('',#16475) ;
#4086 = VERTEX_POINT('',#16479) ;
#4087 = VERTEX_POINT('',#16489) ;
#4088 = VERTEX_POINT('',#16493) ;
#4089 = VERTEX_POINT('',#16503) ;
#4090 = VERTEX_POINT('',#16507) ;
#4091 = VERTEX_POINT('',#16517) ;
#4092 = VERTEX_POINT('',#16521) ;
#4093 = VERTEX_POINT('',#16531) ;
#4094 = VERTEX_POINT('',#16535) ;
#4095 = VERTEX_POINT('',#16545) ;
#4096 = VERTEX_POINT('',#16549) ;
#4097 = VERTEX_POINT('',#16559) ;
#4098 = VERTEX_POINT('',#16563) ;
#4099 = VERTEX_POINT('',#16573) ;
#4100 = VERTEX_POINT('',#16577) ;
#4101 = VERTEX_POINT('',#16587) ;
#4102 = VERTEX_POINT('',#16591) ;
#4103 = VERTEX_POINT('',#16601) ;
#4104 = VERTEX_POINT('',#16605) ;
#4105 = VERTEX_POINT('',#16617) ;
#4106 = VERTEX_POINT('',#16621) ;
#4107 = VERTEX_POINT('',#16624) ;
#4108 = VERTEX_POINT('',#16625) ;
#4109 = VERTEX_POINT('',#16629) ;
#4110 = VERTEX_POINT('',#16631) ;
#4111 = VERTEX_POINT('',#16635) ;
#4112 = VERTEX_POINT('',#16639) ;
#4113 = VERTEX_POINT('',#16641) ;
#4114 = VERTEX_POINT('',#16645) ;
#4115 = VERTEX_POINT('',#16649) ;
#4116 = VERTEX_POINT('',#16651) ;
#4117 = VERTEX_POINT('',#16655) ;
#4118 = VERTEX_POINT('',#16659) ;
#4119 = VERTEX_POINT('',#16661) ;
#4120 = VERTEX_POINT('',#16665) ;
#4121 = VERTEX_POINT('',#16669) ;
#4122 = VERTEX_POINT('',#16671) ;
#4123 = VERTEX_POINT('',#16676) ;
#4124 = VERTEX_POINT('',#16680) ;
#4125 = VERTEX_POINT('',#16686) ;
#4126 = VERTEX_POINT('',#16688) ;
#4127 = VERTEX_POINT('',#16692) ;
#4128 = VERTEX_POINT('',#16694) ;
#4129 = VERTEX_POINT('',#16698) ;
#4130 = VERTEX_POINT('',#16700) ;
#4131 = VERTEX_POINT('',#16704) ;
#4132 = VERTEX_POINT('',#16706) ;
#4133 = VERTEX_POINT('',#16710) ;
#4134 = VERTEX_POINT('',#16712) ;
#4135 = VERTEX_POINT('',#16716) ;
#4136 = VERTEX_POINT('',#16718) ;
#4137 = VERTEX_POINT('',#16723) ;
#4138 = VERTEX_POINT('',#16725) ;
#4139 = VERTEX_POINT('',#16730) ;
#4140 = VERTEX_POINT('',#16735) ;
#4141 = VERTEX_POINT('',#16748) ;
#4142 = VERTEX_POINT('',#16749) ;
#4143 = VERTEX_POINT('',#16765) ;
#4144 = VERTEX_POINT('',#16774) ;
#4145 = VERTEX_POINT('',#16776) ;
#4146 = VERTEX_POINT('',#16779) ;
#4147 = VERTEX_POINT('',#16783) ;
#4148 = VERTEX_POINT('',#16786) ;
#4149 = VERTEX_POINT('',#16790) ;
#4150 = VERTEX_POINT('',#16794) ;
#4151 = VERTEX_POINT('',#16798) ;
#4152 = VERTEX_POINT('',#16802) ;
#4153 = VERTEX_POINT('',#16809) ;
#4154 = VERTEX_POINT('',#16811) ;
#4155 = VERTEX_POINT('',#16815) ;
#4156 = VERTEX_POINT('',#16816) ;
#4157 = VERTEX_POINT('',#16818) ;
#4158 = VERTEX_POINT('',#16820) ;
#4159 = VERTEX_POINT('',#16824) ;
#4160 = VERTEX_POINT('',#16826) ;
#4161 = VERTEX_POINT('',#16830) ;
#4162 = VERTEX_POINT('',#16832) ;
#4163 = VERTEX_POINT('',#16836) ;
#4164 = VERTEX_POINT('',#16838) ;
#4165 = VERTEX_POINT('',#16840) ;
#4166 = VERTEX_POINT('',#16842) ;
#4167 = VERTEX_POINT('',#16845) ;
#4168 = VERTEX_POINT('',#16848) ;
#4169 = VERTEX_POINT('',#16852) ;
#4170 = VERTEX_POINT('',#16854) ;
#4171 = VERTEX_POINT('',#16858) ;
#4172 = VERTEX_POINT('',#16864) ;
#4173 = EDGE_CURVE('',#3398,#3398,#3120,.T.) ;
#4174 = EDGE_CURVE('',#3398,#3399,#1996,.T.) ;
#4175 = EDGE_CURVE('',#3399,#3399,#3121,.T.) ;
#4176 = EDGE_CURVE('',#3399,#3400,#1997,.T.) ;
#4177 = EDGE_CURVE('',#3400,#3401,#3122,.T.) ;
#4178 = EDGE_CURVE('',#3401,#3400,#3123,.T.) ;
#4179 = EDGE_CURVE('',#3402,#3402,#3124,.T.) ;
#4180 = EDGE_CURVE('',#3403,#3401,#1998,.T.) ;
#4181 = EDGE_CURVE('',#3404,#3404,#3125,.T.) ;
#4182 = EDGE_CURVE('',#3404,#3405,#1999,.T.) ;
#4183 = EDGE_CURVE('',#3405,#3405,#3126,.T.) ;
#4184 = EDGE_CURVE('',#3405,#3406,#2000,.T.) ;
#4185 = EDGE_CURVE('',#3406,#3407,#3127,.T.) ;
#4186 = EDGE_CURVE('',#3407,#3406,#3128,.T.) ;
#4187 = EDGE_CURVE('',#3408,#3408,#3129,.T.) ;
#4188 = EDGE_CURVE('',#3407,#3409,#2001,.T.) ;
#4189 = EDGE_CURVE('',#3410,#3411,#3130,.T.) ;
#4190 = EDGE_CURVE('',#3412,#3410,#2002,.T.) ;
#4191 = EDGE_CURVE('',#3411,#3412,#3131,.T.) ;
#4192 = EDGE_CURVE('',#3413,#3410,#2003,.T.) ;
#4193 = EDGE_CURVE('',#3413,#3414,#2004,.T.) ;
#4194 = EDGE_CURVE('',#3412,#3414,#2005,.T.) ;
#4195 = EDGE_CURVE('',#3414,#3415,#3132,.T.) ;
#4196 = EDGE_CURVE('',#3415,#3413,#3133,.T.) ;
#4197 = EDGE_CURVE('',#3416,#3417,#3134,.T.) ;
#4198 = EDGE_CURVE('',#3416,#3417,#2006,.T.) ;
#4199 = EDGE_CURVE('',#3418,#3416,#2007,.T.) ;
#4200 = EDGE_CURVE('',#3418,#3419,#2008,.T.) ;
#4201 = EDGE_CURVE('',#3417,#3419,#2009,.T.) ;
#4202 = EDGE_CURVE('',#3419,#3418,#3135,.T.) ;
#4203 = EDGE_CURVE('',#3420,#3421,#443,.T.) ;
#4204 = EDGE_CURVE('',#3422,#3420,#3136,.T.) ;
#4205 = EDGE_CURVE('',#3423,#3422,#444,.T.) ;
#4206 = EDGE_CURVE('',#3424,#3423,#2010,.T.) ;
#4207 = EDGE_CURVE('',#3425,#3424,#445,.T.) ;
#4208 = EDGE_CURVE('',#3426,#3425,#3137,.T.) ;
#4209 = EDGE_CURVE('',#3427,#3426,#446,.T.) ;
#4210 = EDGE_CURVE('',#3421,#3427,#2011,.T.) ;
#4211 = EDGE_CURVE('',#3428,#3429,#447,.T.) ;
#4212 = EDGE_CURVE('',#3430,#3428,#3138,.T.) ;
#4213 = EDGE_CURVE('',#3431,#3430,#448,.T.) ;
#4214 = EDGE_CURVE('',#3432,#3431,#2012,.T.) ;
#4215 = EDGE_CURVE('',#3433,#3432,#449,.T.) ;
#4216 = EDGE_CURVE('',#3434,#3433,#3139,.T.) ;
#4217 = EDGE_CURVE('',#3435,#3434,#450,.T.) ;
#4218 = EDGE_CURVE('',#3429,#3435,#2013,.T.) ;
#4219 = EDGE_CURVE('',#3436,#3437,#451,.T.) ;
#4220 = EDGE_CURVE('',#3438,#3436,#2014,.T.) ;
#4221 = EDGE_CURVE('',#3439,#3438,#452,.T.) ;
#4222 = EDGE_CURVE('',#3440,#3439,#3140,.T.) ;
#4223 = EDGE_CURVE('',#3441,#3440,#453,.T.) ;
#4224 = EDGE_CURVE('',#3442,#3441,#2015,.T.) ;
#4225 = EDGE_CURVE('',#3443,#3442,#454,.T.) ;
#4226 = EDGE_CURVE('',#3437,#3443,#3141,.T.) ;
#4227 = EDGE_CURVE('',#3444,#3445,#455,.T.) ;
#4228 = EDGE_CURVE('',#3446,#3444,#2016,.T.) ;
#4229 = EDGE_CURVE('',#3447,#3446,#456,.T.) ;
#4230 = EDGE_CURVE('',#3448,#3447,#3142,.T.) ;
#4231 = EDGE_CURVE('',#3449,#3448,#457,.T.) ;
#4232 = EDGE_CURVE('',#3450,#3449,#2017,.T.) ;
#4233 = EDGE_CURVE('',#3451,#3450,#458,.T.) ;
#4234 = EDGE_CURVE('',#3445,#3451,#3143,.T.) ;
#4235 = EDGE_CURVE('',#3442,#3444,#3144,.T.) ;
#4236 = EDGE_CURVE('',#3443,#3445,#3145,.T.) ;
#4237 = EDGE_CURVE('',#3429,#3436,#3146,.T.) ;
#4238 = EDGE_CURVE('',#3428,#3437,#3147,.T.) ;
#4239 = EDGE_CURVE('',#3451,#3422,#3148,.T.) ;
#4240 = EDGE_CURVE('',#3450,#3423,#3149,.T.) ;
#4241 = EDGE_CURVE('',#3421,#3431,#3150,.T.) ;
#4242 = EDGE_CURVE('',#3420,#3430,#3151,.T.) ;
#4243 = EDGE_CURVE('',#3441,#3446,#3152,.T.) ;
#4244 = EDGE_CURVE('',#3435,#3438,#3153,.T.) ;
#4245 = EDGE_CURVE('',#3449,#3424,#3154,.T.) ;
#4246 = EDGE_CURVE('',#3427,#3432,#3155,.T.) ;
#4247 = EDGE_CURVE('',#3440,#3447,#3156,.T.) ;
#4248 = EDGE_CURVE('',#3434,#3439,#3157,.T.) ;
#4249 = EDGE_CURVE('',#3448,#3425,#3158,.T.) ;
#4250 = EDGE_CURVE('',#3426,#3433,#3159,.T.) ;
#4251 = EDGE_CURVE('',#3452,#3452,#3160,.T.) ;
#4252 = EDGE_CURVE('',#3453,#3453,#3161,.T.) ;
#4253 = EDGE_CURVE('',#3453,#3408,#2018,.T.) ;
#4254 = EDGE_CURVE('',#3452,#3453,#2019,.T.) ;
#4255 = EDGE_CURVE('',#3454,#3454,#3162,.T.) ;
#4256 = EDGE_CURVE('',#3455,#3455,#3163,.T.) ;
#4257 = EDGE_CURVE('',#3455,#3411,#2020,.T.) ;
#4258 = EDGE_CURVE('',#3415,#3454,#2021,.T.) ;
#4259 = EDGE_CURVE('',#3402,#3455,#2022,.T.) ;
#4260 = EDGE_CURVE('',#3456,#3457,#459,.T.) ;
#4261 = EDGE_CURVE('',#3456,#3458,#2023,.T.) ;
#4262 = EDGE_CURVE('',#3458,#3459,#460,.T.) ;
#4263 = EDGE_CURVE('',#3457,#3459,#2024,.T.) ;
#4264 = EDGE_CURVE('',#3457,#3460,#461,.T.) ;
#4265 = EDGE_CURVE('',#3459,#3461,#462,.T.) ;
#4266 = EDGE_CURVE('',#3460,#3461,#2025,.T.) ;
#4267 = EDGE_CURVE('',#3460,#3462,#463,.T.) ;
#4268 = EDGE_CURVE('',#3461,#3463,#464,.T.) ;
#4269 = EDGE_CURVE('',#3462,#3463,#2026,.T.) ;
#4270 = EDGE_CURVE('',#3462,#3464,#465,.T.) ;
#4271 = EDGE_CURVE('',#3463,#3465,#466,.T.) ;
#4272 = EDGE_CURVE('',#3464,#3465,#2027,.T.) ;
#4273 = EDGE_CURVE('',#3466,#3467,#467,.T.) ;
#4274 = EDGE_CURVE('',#3466,#3468,#2028,.T.) ;
#4275 = EDGE_CURVE('',#3468,#3469,#468,.T.) ;
#4276 = EDGE_CURVE('',#3467,#3469,#2029,.T.) ;
#4277 = EDGE_CURVE('',#3467,#3470,#469,.T.) ;
#4278 = EDGE_CURVE('',#3469,#3471,#470,.T.) ;
#4279 = EDGE_CURVE('',#3470,#3471,#2030,.T.) ;
#4280 = EDGE_CURVE('',#3470,#3472,#471,.T.) ;
#4281 = EDGE_CURVE('',#3471,#3473,#472,.T.) ;
#4282 = EDGE_CURVE('',#3472,#3473,#2031,.T.) ;
#4283 = EDGE_CURVE('',#3472,#3474,#473,.T.) ;
#4284 = EDGE_CURVE('',#3473,#3475,#474,.T.) ;
#4285 = EDGE_CURVE('',#3474,#3475,#2032,.T.) ;
#4286 = EDGE_CURVE('',#3474,#3476,#475,.T.) ;
#4287 = EDGE_CURVE('',#3475,#3477,#476,.T.) ;
#4288 = EDGE_CURVE('',#3476,#3477,#2033,.T.) ;
#4289 = EDGE_CURVE('',#3476,#3478,#477,.T.) ;
#4290 = EDGE_CURVE('',#3477,#3479,#478,.T.) ;
#4291 = EDGE_CURVE('',#3478,#3479,#2034,.T.) ;
#4292 = EDGE_CURVE('',#3478,#3480,#479,.T.) ;
#4293 = EDGE_CURVE('',#3479,#3481,#480,.T.) ;
#4294 = EDGE_CURVE('',#3480,#3481,#2035,.T.) ;
#4295 = EDGE_CURVE('',#3480,#3482,#481,.T.) ;
#4296 = EDGE_CURVE('',#3481,#3483,#482,.T.) ;
#4297 = EDGE_CURVE('',#3482,#3483,#2036,.T.) ;
#4298 = EDGE_CURVE('',#3482,#3484,#483,.T.) ;
#4299 = EDGE_CURVE('',#3483,#3485,#484,.T.) ;
#4300 = EDGE_CURVE('',#3484,#3485,#2037,.T.) ;
#4301 = EDGE_CURVE('',#3464,#3486,#485,.T.) ;
#4302 = EDGE_CURVE('',#3465,#3487,#486,.T.) ;
#4303 = EDGE_CURVE('',#3486,#3487,#2038,.T.) ;
#4304 = EDGE_CURVE('',#3488,#3456,#487,.T.) ;
#4305 = EDGE_CURVE('',#3488,#3489,#2039,.T.) ;
#4306 = EDGE_CURVE('',#3489,#3458,#488,.T.) ;
#4307 = EDGE_CURVE('',#3490,#3488,#489,.T.) ;
#4308 = EDGE_CURVE('',#3490,#3491,#2040,.T.) ;
#4309 = EDGE_CURVE('',#3491,#3489,#490,.T.) ;
#4310 = EDGE_CURVE('',#3492,#3490,#491,.T.) ;
#4311 = EDGE_CURVE('',#3492,#3493,#2041,.T.) ;
#4312 = EDGE_CURVE('',#3493,#3491,#492,.T.) ;
#4313 = EDGE_CURVE('',#3486,#3492,#493,.T.) ;
#4314 = EDGE_CURVE('',#3487,#3493,#494,.T.) ;
#4315 = EDGE_CURVE('',#3484,#3494,#495,.T.) ;
#4316 = EDGE_CURVE('',#3485,#3495,#496,.T.) ;
#4317 = EDGE_CURVE('',#3494,#3495,#2042,.T.) ;
#4318 = EDGE_CURVE('',#3496,#3466,#497,.T.) ;
#4319 = EDGE_CURVE('',#3496,#3497,#2043,.T.) ;
#4320 = EDGE_CURVE('',#3497,#3468,#498,.T.) ;
#4321 = EDGE_CURVE('',#3498,#3496,#499,.T.) ;
#4322 = EDGE_CURVE('',#3498,#3499,#2044,.T.) ;
#4323 = EDGE_CURVE('',#3499,#3497,#500,.T.) ;
#4324 = EDGE_CURVE('',#3500,#3498,#501,.T.) ;
#4325 = EDGE_CURVE('',#3500,#3501,#2045,.T.) ;
#4326 = EDGE_CURVE('',#3501,#3499,#502,.T.) ;
#4327 = EDGE_CURVE('',#3502,#3500,#503,.T.) ;
#4328 = EDGE_CURVE('',#3502,#3503,#2046,.T.) ;
#4329 = EDGE_CURVE('',#3503,#3501,#504,.T.) ;
#4330 = EDGE_CURVE('',#3504,#3502,#505,.T.) ;
#4331 = EDGE_CURVE('',#3504,#3505,#2047,.T.) ;
#4332 = EDGE_CURVE('',#3505,#3503,#506,.T.) ;
#4333 = EDGE_CURVE('',#3506,#3504,#507,.T.) ;
#4334 = EDGE_CURVE('',#3506,#3507,#2048,.T.) ;
#4335 = EDGE_CURVE('',#3507,#3505,#508,.T.) ;
#4336 = EDGE_CURVE('',#3508,#3506,#509,.T.) ;
#4337 = EDGE_CURVE('',#3508,#3509,#2049,.T.) ;
#4338 = EDGE_CURVE('',#3509,#3507,#510,.T.) ;
#4339 = EDGE_CURVE('',#3510,#3508,#319,.T.) ;
#4340 = EDGE_CURVE('',#3510,#3511,#2050,.T.) ;
#4341 = EDGE_CURVE('',#3511,#3509,#2051,.T.) ;
#4342 = EDGE_CURVE('',#3494,#3510,#511,.T.) ;
#4343 = EDGE_CURVE('',#3495,#3511,#512,.T.) ;
#4344 = EDGE_CURVE('',#3512,#3513,#513,.T.) ;
#4345 = EDGE_CURVE('',#3512,#3514,#2052,.T.) ;
#4346 = EDGE_CURVE('',#3514,#3515,#514,.T.) ;
#4347 = EDGE_CURVE('',#3513,#3515,#2053,.T.) ;
#4348 = EDGE_CURVE('',#3513,#3516,#3164,.T.) ;
#4349 = EDGE_CURVE('',#3515,#3517,#2054,.T.) ;
#4350 = EDGE_CURVE('',#3516,#3517,#2055,.T.) ;
#4351 = EDGE_CURVE('',#3516,#3518,#515,.T.) ;
#4352 = EDGE_CURVE('',#3517,#3519,#516,.T.) ;
#4353 = EDGE_CURVE('',#3518,#3519,#2056,.T.) ;
#4354 = EDGE_CURVE('',#3518,#3520,#517,.T.) ;
#4355 = EDGE_CURVE('',#3519,#3521,#518,.T.) ;
#4356 = EDGE_CURVE('',#3520,#3521,#2057,.T.) ;
#4357 = EDGE_CURVE('',#3520,#3522,#2058,.T.) ;
#4358 = EDGE_CURVE('',#3521,#3523,#2059,.T.) ;
#4359 = EDGE_CURVE('',#3522,#3523,#2060,.T.) ;
#4360 = EDGE_CURVE('',#3524,#3512,#519,.T.) ;
#4361 = EDGE_CURVE('',#3524,#3525,#2061,.T.) ;
#4362 = EDGE_CURVE('',#3525,#3514,#520,.T.) ;
#4363 = EDGE_CURVE('',#3526,#3524,#3165,.T.) ;
#4364 = EDGE_CURVE('',#3526,#3527,#2062,.T.) ;
#4365 = EDGE_CURVE('',#3527,#3525,#2063,.T.) ;
#4366 = EDGE_CURVE('',#3528,#3526,#2064,.T.) ;
#4367 = EDGE_CURVE('',#3528,#3529,#2065,.T.) ;
#4368 = EDGE_CURVE('',#3529,#3527,#2066,.T.) ;
#4369 = EDGE_CURVE('',#3522,#3528,#3166,.T.) ;
#4370 = EDGE_CURVE('',#3523,#3529,#2067,.T.) ;
#4371 = EDGE_CURVE('',#3530,#3530,#3167,.T.) ;
#4372 = EDGE_CURVE('',#3530,#3531,#2068,.T.) ;
#4373 = EDGE_CURVE('',#3531,#3531,#3168,.T.) ;
#4374 = EDGE_CURVE('',#3532,#3533,#3169,.T.) ;
#4375 = EDGE_CURVE('',#3533,#3534,#2069,.T.) ;
#4376 = EDGE_CURVE('',#3534,#3535,#3170,.T.) ;
#4377 = EDGE_CURVE('',#3535,#3536,#2070,.T.) ;
#4378 = EDGE_CURVE('',#3536,#3537,#320,.T.) ;
#4379 = EDGE_CURVE('',#3537,#3538,#521,.T.) ;
#4380 = EDGE_CURVE('',#3538,#3539,#522,.T.) ;
#4381 = EDGE_CURVE('',#3539,#3540,#321,.T.) ;
#4382 = EDGE_CURVE('',#3540,#3541,#2071,.T.) ;
#4383 = EDGE_CURVE('',#3541,#3542,#3171,.T.) ;
#4384 = EDGE_CURVE('',#3542,#3543,#2072,.T.) ;
#4385 = EDGE_CURVE('',#3543,#3544,#3172,.T.) ;
#4386 = EDGE_CURVE('',#3544,#3545,#322,.T.) ;
#4387 = EDGE_CURVE('',#3545,#3546,#2073,.T.) ;
#4388 = EDGE_CURVE('',#3546,#3532,#323,.T.) ;
#4389 = EDGE_CURVE('',#3547,#3548,#523,.T.) ;
#4390 = EDGE_CURVE('',#3548,#3549,#524,.T.) ;
#4391 = EDGE_CURVE('',#3549,#3550,#324,.T.) ;
#4392 = EDGE_CURVE('',#3550,#3551,#525,.T.) ;
#4393 = EDGE_CURVE('',#3551,#3552,#526,.T.) ;
#4394 = EDGE_CURVE('',#3552,#3553,#527,.T.) ;
#4395 = EDGE_CURVE('',#3553,#3554,#528,.T.) ;
#4396 = EDGE_CURVE('',#3554,#3555,#529,.T.) ;
#4397 = EDGE_CURVE('',#3555,#3556,#530,.T.) ;
#4398 = EDGE_CURVE('',#3556,#3557,#531,.T.) ;
#4399 = EDGE_CURVE('',#3557,#3558,#532,.T.) ;
#4400 = EDGE_CURVE('',#3558,#3559,#533,.T.) ;
#4401 = EDGE_CURVE('',#3559,#3560,#534,.T.) ;
#4402 = EDGE_CURVE('',#3560,#3561,#535,.T.) ;
#4403 = EDGE_CURVE('',#3561,#3562,#536,.T.) ;
#4404 = EDGE_CURVE('',#3562,#3563,#537,.T.) ;
#4405 = EDGE_CURVE('',#3563,#3564,#538,.T.) ;
#4406 = EDGE_CURVE('',#3564,#3565,#539,.T.) ;
#4407 = EDGE_CURVE('',#3565,#3566,#540,.T.) ;
#4408 = EDGE_CURVE('',#3566,#3567,#541,.T.) ;
#4409 = EDGE_CURVE('',#3567,#3568,#542,.T.) ;
#4410 = EDGE_CURVE('',#3568,#3569,#325,.T.) ;
#4411 = EDGE_CURVE('',#3569,#3570,#543,.T.) ;
#4412 = EDGE_CURVE('',#3570,#3571,#544,.T.) ;
#4413 = EDGE_CURVE('',#3571,#3572,#545,.T.) ;
#4414 = EDGE_CURVE('',#3572,#3573,#546,.T.) ;
#4415 = EDGE_CURVE('',#3573,#3574,#547,.T.) ;
#4416 = EDGE_CURVE('',#3574,#3575,#548,.T.) ;
#4417 = EDGE_CURVE('',#3575,#3576,#549,.T.) ;
#4418 = EDGE_CURVE('',#3576,#3577,#550,.T.) ;
#4419 = EDGE_CURVE('',#3577,#3578,#551,.T.) ;
#4420 = EDGE_CURVE('',#3578,#3579,#552,.T.) ;
#4421 = EDGE_CURVE('',#3579,#3580,#553,.T.) ;
#4422 = EDGE_CURVE('',#3580,#3581,#554,.T.) ;
#4423 = EDGE_CURVE('',#3581,#3547,#555,.T.) ;
#4424 = EDGE_CURVE('',#3582,#3583,#556,.T.) ;
#4425 = EDGE_CURVE('',#3583,#3584,#3173,.T.) ;
#4426 = EDGE_CURVE('',#3584,#3585,#2074,.T.) ;
#4427 = EDGE_CURVE('',#3585,#3586,#3174,.T.) ;
#4428 = EDGE_CURVE('',#3586,#3587,#557,.T.) ;
#4429 = EDGE_CURVE('',#3587,#3588,#558,.T.) ;
#4430 = EDGE_CURVE('',#3588,#3589,#559,.T.) ;
#4431 = EDGE_CURVE('',#3589,#3590,#560,.T.) ;
#4432 = EDGE_CURVE('',#3590,#3591,#561,.T.) ;
#4433 = EDGE_CURVE('',#3591,#3592,#562,.T.) ;
#4434 = EDGE_CURVE('',#3592,#3593,#3175,.T.) ;
#4435 = EDGE_CURVE('',#3593,#3594,#2075,.T.) ;
#4436 = EDGE_CURVE('',#3594,#3595,#3176,.T.) ;
#4437 = EDGE_CURVE('',#3595,#3596,#563,.T.) ;
#4438 = EDGE_CURVE('',#3596,#3597,#564,.T.) ;
#4439 = EDGE_CURVE('',#3597,#3598,#565,.T.) ;
#4440 = EDGE_CURVE('',#3598,#3582,#566,.T.) ;
#4441 = EDGE_CURVE('',#3599,#3600,#3177,.T.) ;
#4442 = EDGE_CURVE('',#3600,#3601,#2076,.T.) ;
#4443 = EDGE_CURVE('',#3601,#3602,#3178,.T.) ;
#4444 = EDGE_CURVE('',#3602,#3603,#2077,.T.) ;
#4445 = EDGE_CURVE('',#3603,#3604,#326,.T.) ;
#4446 = EDGE_CURVE('',#3604,#3605,#567,.T.) ;
#4447 = EDGE_CURVE('',#3605,#3606,#568,.T.) ;
#4448 = EDGE_CURVE('',#3606,#3607,#327,.T.) ;
#4449 = EDGE_CURVE('',#3607,#3608,#2078,.T.) ;
#4450 = EDGE_CURVE('',#3608,#3609,#3179,.T.) ;
#4451 = EDGE_CURVE('',#3609,#3610,#2079,.T.) ;
#4452 = EDGE_CURVE('',#3610,#3611,#3180,.T.) ;
#4453 = EDGE_CURVE('',#3611,#3612,#328,.T.) ;
#4454 = EDGE_CURVE('',#3612,#3613,#2080,.T.) ;
#4455 = EDGE_CURVE('',#3613,#3599,#329,.T.) ;
#4456 = EDGE_CURVE('',#3614,#3615,#3181,.T.) ;
#4457 = EDGE_CURVE('',#3615,#3616,#2081,.T.) ;
#4458 = EDGE_CURVE('',#3616,#3617,#3182,.T.) ;
#4459 = EDGE_CURVE('',#3617,#3614,#2082,.T.) ;
#4460 = EDGE_CURVE('',#3618,#3619,#3183,.T.) ;
#4461 = EDGE_CURVE('',#3619,#3620,#2083,.T.) ;
#4462 = EDGE_CURVE('',#3620,#3621,#3184,.T.) ;
#4463 = EDGE_CURVE('',#3621,#3618,#2084,.T.) ;
#4464 = EDGE_CURVE('',#3620,#3622,#2085,.T.) ;
#4465 = EDGE_CURVE('',#3622,#3623,#2086,.T.) ;
#4466 = EDGE_CURVE('',#3621,#3623,#2087,.T.) ;
#4467 = EDGE_CURVE('',#3623,#3624,#2088,.T.) ;
#4468 = EDGE_CURVE('',#3618,#3624,#2089,.T.) ;
#4469 = EDGE_CURVE('',#3624,#3625,#2090,.T.) ;
#4470 = EDGE_CURVE('',#3619,#3625,#2091,.T.) ;
#4471 = EDGE_CURVE('',#3625,#3622,#2092,.T.) ;
#4472 = EDGE_CURVE('',#3616,#3626,#2093,.T.) ;
#4473 = EDGE_CURVE('',#3626,#3627,#2094,.T.) ;
#4474 = EDGE_CURVE('',#3617,#3627,#2095,.T.) ;
#4475 = EDGE_CURVE('',#3627,#3628,#2096,.T.) ;
#4476 = EDGE_CURVE('',#3614,#3628,#2097,.T.) ;
#4477 = EDGE_CURVE('',#3628,#3629,#2098,.T.) ;
#4478 = EDGE_CURVE('',#3615,#3629,#2099,.T.) ;
#4479 = EDGE_CURVE('',#3629,#3626,#2100,.T.) ;
#4480 = EDGE_CURVE('',#3607,#3630,#2101,.T.) ;
#4481 = EDGE_CURVE('',#3630,#3631,#2102,.T.) ;
#4482 = EDGE_CURVE('',#3608,#3631,#2103,.T.) ;
#4483 = EDGE_CURVE('',#3631,#3632,#2104,.T.) ;
#4484 = EDGE_CURVE('',#3609,#3632,#2105,.T.) ;
#4485 = EDGE_CURVE('',#3632,#3633,#2106,.T.) ;
#4486 = EDGE_CURVE('',#3610,#3633,#2107,.T.) ;
#4487 = EDGE_CURVE('',#3633,#3634,#2108,.T.) ;
#4488 = EDGE_CURVE('',#3611,#3634,#2109,.T.) ;
#4489 = EDGE_CURVE('',#3634,#3635,#2110,.T.) ;
#4490 = EDGE_CURVE('',#3612,#3635,#2111,.T.) ;
#4491 = EDGE_CURVE('',#3635,#3636,#2112,.T.) ;
#4492 = EDGE_CURVE('',#3613,#3636,#2113,.T.) ;
#4493 = EDGE_CURVE('',#3636,#3637,#2114,.T.) ;
#4494 = EDGE_CURVE('',#3599,#3637,#2115,.T.) ;
#4495 = EDGE_CURVE('',#3637,#3638,#2116,.T.) ;
#4496 = EDGE_CURVE('',#3600,#3638,#2117,.T.) ;
#4497 = EDGE_CURVE('',#3606,#3639,#2118,.T.) ;
#4498 = EDGE_CURVE('',#3639,#3630,#2119,.T.) ;
#4499 = EDGE_CURVE('',#3605,#3640,#2120,.T.) ;
#4500 = EDGE_CURVE('',#3640,#3639,#569,.T.) ;
#4501 = EDGE_CURVE('',#3604,#3641,#2121,.T.) ;
#4502 = EDGE_CURVE('',#3641,#3640,#570,.T.) ;
#4503 = EDGE_CURVE('',#3603,#3642,#2122,.T.) ;
#4504 = EDGE_CURVE('',#3642,#3641,#2123,.T.) ;
#4505 = EDGE_CURVE('',#3602,#3643,#2124,.T.) ;
#4506 = EDGE_CURVE('',#3643,#3642,#2125,.T.) ;
#4507 = EDGE_CURVE('',#3601,#3644,#2126,.T.) ;
#4508 = EDGE_CURVE('',#3644,#3643,#2127,.T.) ;
#4509 = EDGE_CURVE('',#3638,#3644,#2128,.T.) ;
#4510 = EDGE_CURVE('',#3591,#3645,#2129,.T.) ;
#4511 = EDGE_CURVE('',#3645,#3646,#571,.T.) ;
#4512 = EDGE_CURVE('',#3592,#3646,#2130,.T.) ;
#4513 = EDGE_CURVE('',#3646,#3647,#2131,.T.) ;
#4514 = EDGE_CURVE('',#3593,#3647,#2132,.T.) ;
#4515 = EDGE_CURVE('',#3647,#3648,#2133,.T.) ;
#4516 = EDGE_CURVE('',#3594,#3648,#2134,.T.) ;
#4517 = EDGE_CURVE('',#3648,#3649,#2135,.T.) ;
#4518 = EDGE_CURVE('',#3595,#3649,#2136,.T.) ;
#4519 = EDGE_CURVE('',#3649,#3650,#572,.T.) ;
#4520 = EDGE_CURVE('',#3596,#3650,#2137,.T.) ;
#4521 = EDGE_CURVE('',#3650,#3651,#573,.T.) ;
#4522 = EDGE_CURVE('',#3597,#3651,#2138,.T.) ;
#4523 = EDGE_CURVE('',#3651,#3652,#574,.T.) ;
#4524 = EDGE_CURVE('',#3598,#3652,#2139,.T.) ;
#4525 = EDGE_CURVE('',#3652,#3653,#575,.T.) ;
#4526 = EDGE_CURVE('',#3582,#3653,#2140,.T.) ;
#4527 = EDGE_CURVE('',#3653,#3654,#576,.T.) ;
#4528 = EDGE_CURVE('',#3583,#3654,#2141,.T.) ;
#4529 = EDGE_CURVE('',#3590,#3655,#2142,.T.) ;
#4530 = EDGE_CURVE('',#3655,#3645,#577,.T.) ;
#4531 = EDGE_CURVE('',#3589,#3656,#2143,.T.) ;
#4532 = EDGE_CURVE('',#3656,#3655,#578,.T.) ;
#4533 = EDGE_CURVE('',#3588,#3657,#2144,.T.) ;
#4534 = EDGE_CURVE('',#3657,#3656,#579,.T.) ;
#4535 = EDGE_CURVE('',#3587,#3658,#2145,.T.) ;
#4536 = EDGE_CURVE('',#3658,#3657,#580,.T.) ;
#4537 = EDGE_CURVE('',#3586,#3659,#2146,.T.) ;
#4538 = EDGE_CURVE('',#3659,#3658,#581,.T.) ;
#4539 = EDGE_CURVE('',#3585,#3660,#2147,.T.) ;
#4540 = EDGE_CURVE('',#3660,#3659,#2148,.T.) ;
#4541 = EDGE_CURVE('',#3584,#3661,#2149,.T.) ;
#4542 = EDGE_CURVE('',#3661,#3660,#2150,.T.) ;
#4543 = EDGE_CURVE('',#3654,#3661,#2151,.T.) ;
#4544 = EDGE_CURVE('',#3565,#3662,#2152,.T.) ;
#4545 = EDGE_CURVE('',#3662,#3663,#582,.T.) ;
#4546 = EDGE_CURVE('',#3566,#3663,#2153,.T.) ;
#4547 = EDGE_CURVE('',#3663,#3664,#583,.T.) ;
#4548 = EDGE_CURVE('',#3567,#3664,#2154,.T.) ;
#4549 = EDGE_CURVE('',#3664,#3665,#584,.T.) ;
#4550 = EDGE_CURVE('',#3568,#3665,#2155,.T.) ;
#4551 = EDGE_CURVE('',#3665,#3666,#2156,.T.) ;
#4552 = EDGE_CURVE('',#3569,#3666,#2157,.T.) ;
#4553 = EDGE_CURVE('',#3666,#3667,#585,.T.) ;
#4554 = EDGE_CURVE('',#3570,#3667,#2158,.T.) ;
#4555 = EDGE_CURVE('',#3667,#3668,#586,.T.) ;
#4556 = EDGE_CURVE('',#3571,#3668,#2159,.T.) ;
#4557 = EDGE_CURVE('',#3668,#3669,#587,.T.) ;
#4558 = EDGE_CURVE('',#3572,#3669,#2160,.T.) ;
#4559 = EDGE_CURVE('',#3669,#3670,#588,.T.) ;
#4560 = EDGE_CURVE('',#3573,#3670,#2161,.T.) ;
#4561 = EDGE_CURVE('',#3670,#3671,#589,.T.) ;
#4562 = EDGE_CURVE('',#3574,#3671,#2162,.T.) ;
#4563 = EDGE_CURVE('',#3671,#3672,#590,.T.) ;
#4564 = EDGE_CURVE('',#3575,#3672,#2163,.T.) ;
#4565 = EDGE_CURVE('',#3672,#3673,#591,.T.) ;
#4566 = EDGE_CURVE('',#3576,#3673,#2164,.T.) ;
#4567 = EDGE_CURVE('',#3673,#3674,#592,.T.) ;
#4568 = EDGE_CURVE('',#3577,#3674,#2165,.T.) ;
#4569 = EDGE_CURVE('',#3674,#3675,#593,.T.) ;
#4570 = EDGE_CURVE('',#3578,#3675,#2166,.T.) ;
#4571 = EDGE_CURVE('',#3675,#3676,#594,.T.) ;
#4572 = EDGE_CURVE('',#3579,#3676,#2167,.T.) ;
#4573 = EDGE_CURVE('',#3676,#3677,#595,.T.) ;
#4574 = EDGE_CURVE('',#3580,#3677,#2168,.T.) ;
#4575 = EDGE_CURVE('',#3677,#3678,#596,.T.) ;
#4576 = EDGE_CURVE('',#3581,#3678,#2169,.T.) ;
#4577 = EDGE_CURVE('',#3678,#3679,#597,.T.) ;
#4578 = EDGE_CURVE('',#3547,#3679,#2170,.T.) ;
#4579 = EDGE_CURVE('',#3679,#3680,#598,.T.) ;
#4580 = EDGE_CURVE('',#3548,#3680,#2171,.T.) ;
#4581 = EDGE_CURVE('',#3564,#3681,#2172,.T.) ;
#4582 = EDGE_CURVE('',#3681,#3662,#599,.T.) ;
#4583 = EDGE_CURVE('',#3563,#3682,#2173,.T.) ;
#4584 = EDGE_CURVE('',#3682,#3681,#600,.T.) ;
#4585 = EDGE_CURVE('',#3562,#3683,#2174,.T.) ;
#4586 = EDGE_CURVE('',#3683,#3682,#601,.T.) ;
#4587 = EDGE_CURVE('',#3561,#3684,#2175,.T.) ;
#4588 = EDGE_CURVE('',#3684,#3683,#602,.T.) ;
#4589 = EDGE_CURVE('',#3560,#3685,#2176,.T.) ;
#4590 = EDGE_CURVE('',#3685,#3684,#603,.T.) ;
#4591 = EDGE_CURVE('',#3559,#3686,#2177,.T.) ;
#4592 = EDGE_CURVE('',#3686,#3685,#604,.T.) ;
#4593 = EDGE_CURVE('',#3558,#3687,#2178,.T.) ;
#4594 = EDGE_CURVE('',#3687,#3686,#605,.T.) ;
#4595 = EDGE_CURVE('',#3557,#3688,#2179,.T.) ;
#4596 = EDGE_CURVE('',#3688,#3687,#606,.T.) ;
#4597 = EDGE_CURVE('',#3556,#3689,#2180,.T.) ;
#4598 = EDGE_CURVE('',#3689,#3688,#607,.T.) ;
#4599 = EDGE_CURVE('',#3555,#3690,#2181,.T.) ;
#4600 = EDGE_CURVE('',#3690,#3689,#608,.T.) ;
#4601 = EDGE_CURVE('',#3554,#3691,#2182,.T.) ;
#4602 = EDGE_CURVE('',#3691,#3690,#609,.T.) ;
#4603 = EDGE_CURVE('',#3553,#3692,#2183,.T.) ;
#4604 = EDGE_CURVE('',#3692,#3691,#610,.T.) ;
#4605 = EDGE_CURVE('',#3552,#3693,#2184,.T.) ;
#4606 = EDGE_CURVE('',#3693,#3692,#611,.T.) ;
#4607 = EDGE_CURVE('',#3551,#3694,#2185,.T.) ;
#4608 = EDGE_CURVE('',#3694,#3693,#612,.T.) ;
#4609 = EDGE_CURVE('',#3550,#3695,#2186,.T.) ;
#4610 = EDGE_CURVE('',#3695,#3694,#613,.T.) ;
#4611 = EDGE_CURVE('',#3549,#3696,#2187,.T.) ;
#4612 = EDGE_CURVE('',#3696,#3695,#2188,.T.) ;
#4613 = EDGE_CURVE('',#3680,#3696,#614,.T.) ;
#4614 = EDGE_CURVE('',#3540,#3697,#2189,.T.) ;
#4615 = EDGE_CURVE('',#3697,#3698,#2190,.T.) ;
#4616 = EDGE_CURVE('',#3541,#3698,#2191,.T.) ;
#4617 = EDGE_CURVE('',#3698,#3699,#2192,.T.) ;
#4618 = EDGE_CURVE('',#3542,#3699,#2193,.T.) ;
#4619 = EDGE_CURVE('',#3699,#3700,#2194,.T.) ;
#4620 = EDGE_CURVE('',#3543,#3700,#2195,.T.) ;
#4621 = EDGE_CURVE('',#3700,#3701,#2196,.T.) ;
#4622 = EDGE_CURVE('',#3544,#3701,#2197,.T.) ;
#4623 = EDGE_CURVE('',#3701,#3702,#2198,.T.) ;
#4624 = EDGE_CURVE('',#3545,#3702,#2199,.T.) ;
#4625 = EDGE_CURVE('',#3702,#3703,#2200,.T.) ;
#4626 = EDGE_CURVE('',#3546,#3703,#2201,.T.) ;
#4627 = EDGE_CURVE('',#3703,#3704,#2202,.T.) ;
#4628 = EDGE_CURVE('',#3532,#3704,#2203,.T.) ;
#4629 = EDGE_CURVE('',#3704,#3705,#2204,.T.) ;
#4630 = EDGE_CURVE('',#3533,#3705,#2205,.T.) ;
#4631 = EDGE_CURVE('',#3539,#3706,#2206,.T.) ;
#4632 = EDGE_CURVE('',#3706,#3697,#2207,.T.) ;
#4633 = EDGE_CURVE('',#3538,#3707,#2208,.T.) ;
#4634 = EDGE_CURVE('',#3707,#3706,#615,.T.) ;
#4635 = EDGE_CURVE('',#3537,#3708,#2209,.T.) ;
#4636 = EDGE_CURVE('',#3708,#3707,#616,.T.) ;
#4637 = EDGE_CURVE('',#3536,#3709,#2210,.T.) ;
#4638 = EDGE_CURVE('',#3709,#3708,#2211,.T.) ;
#4639 = EDGE_CURVE('',#3535,#3710,#2212,.T.) ;
#4640 = EDGE_CURVE('',#3710,#3709,#2213,.T.) ;
#4641 = EDGE_CURVE('',#3534,#3711,#2214,.T.) ;
#4642 = EDGE_CURVE('',#3711,#3710,#2215,.T.) ;
#4643 = EDGE_CURVE('',#3705,#3711,#2216,.T.) ;
#4644 = EDGE_CURVE('',#3712,#3712,#3185,.T.) ;
#4645 = EDGE_CURVE('',#3712,#3713,#2217,.T.) ;
#4646 = EDGE_CURVE('',#3713,#3713,#3186,.T.) ;
#4647 = EDGE_CURVE('',#3714,#3714,#3187,.T.) ;
#4648 = EDGE_CURVE('',#3715,#3716,#2218,.T.) ;
#4649 = EDGE_CURVE('',#3716,#3717,#3188,.T.) ;
#4650 = EDGE_CURVE('',#3717,#3718,#3189,.T.) ;
#4651 = EDGE_CURVE('',#3718,#3719,#2219,.T.) ;
#4652 = EDGE_CURVE('',#3719,#3715,#3190,.T.) ;
#4653 = EDGE_CURVE('',#3715,#3719,#617,.T.) ;
#4654 = EDGE_CURVE('',#3718,#3716,#618,.T.) ;
#4655 = EDGE_CURVE('',#3715,#3720,#3191,.T.) ;
#4656 = EDGE_CURVE('',#3721,#3720,#619,.T.) ;
#4657 = EDGE_CURVE('',#3721,#3722,#3192,.T.) ;
#4658 = EDGE_CURVE('',#3723,#3722,#620,.T.) ;
#4659 = EDGE_CURVE('',#3723,#3724,#3193,.T.) ;
#4660 = EDGE_CURVE('',#3725,#3724,#621,.T.) ;
#4661 = EDGE_CURVE('',#3725,#3726,#3194,.T.) ;
#4662 = EDGE_CURVE('',#3726,#3727,#3195,.T.) ;
#4663 = EDGE_CURVE('',#3727,#3728,#3196,.T.) ;
#4664 = EDGE_CURVE('',#3728,#3727,#3197,.T.) ;
#4665 = EDGE_CURVE('',#3726,#3719,#3198,.T.) ;
#4666 = EDGE_CURVE('',#3717,#3729,#2220,.T.) ;
#4667 = EDGE_CURVE('',#3729,#3729,#3199,.T.) ;
#4668 = EDGE_CURVE('',#3725,#3730,#2221,.T.) ;
#4669 = EDGE_CURVE('',#3730,#3731,#3200,.T.) ;
#4670 = EDGE_CURVE('',#3731,#3732,#3201,.T.) ;
#4671 = EDGE_CURVE('',#3732,#3724,#2222,.T.) ;
#4672 = EDGE_CURVE('',#3724,#3725,#3202,.T.) ;
#4673 = EDGE_CURVE('',#3732,#3730,#622,.T.) ;
#4674 = EDGE_CURVE('',#3731,#3733,#2223,.T.) ;
#4675 = EDGE_CURVE('',#3733,#3733,#3203,.T.) ;
#4676 = EDGE_CURVE('',#3723,#3734,#2224,.T.) ;
#4677 = EDGE_CURVE('',#3734,#3735,#3204,.T.) ;
#4678 = EDGE_CURVE('',#3735,#3736,#3205,.T.) ;
#4679 = EDGE_CURVE('',#3736,#3722,#2225,.T.) ;
#4680 = EDGE_CURVE('',#3722,#3723,#3206,.T.) ;
#4681 = EDGE_CURVE('',#3736,#3734,#623,.T.) ;
#4682 = EDGE_CURVE('',#3735,#3737,#2226,.T.) ;
#4683 = EDGE_CURVE('',#3737,#3737,#3207,.T.) ;
#4684 = EDGE_CURVE('',#3721,#3738,#2227,.T.) ;
#4685 = EDGE_CURVE('',#3738,#3739,#3208,.T.) ;
#4686 = EDGE_CURVE('',#3739,#3740,#3209,.T.) ;
#4687 = EDGE_CURVE('',#3740,#3720,#2228,.T.) ;
#4688 = EDGE_CURVE('',#3720,#3721,#3210,.T.) ;
#4689 = EDGE_CURVE('',#3740,#3738,#624,.T.) ;
#4690 = EDGE_CURVE('',#3739,#3741,#2229,.T.) ;
#4691 = EDGE_CURVE('',#3741,#3741,#3211,.T.) ;
#4692 = EDGE_CURVE('',#3742,#3742,#3212,.T.) ;
#4693 = EDGE_CURVE('',#3743,#3743,#3213,.T.) ;
#4694 = EDGE_CURVE('',#3744,#3744,#3214,.T.) ;
#4695 = EDGE_CURVE('',#3745,#3745,#3215,.T.) ;
#4696 = EDGE_CURVE('',#3742,#3746,#2230,.T.) ;
#4697 = EDGE_CURVE('',#3746,#3746,#3216,.T.) ;
#4698 = EDGE_CURVE('',#3743,#3747,#2231,.T.) ;
#4699 = EDGE_CURVE('',#3747,#3747,#3217,.T.) ;
#4700 = EDGE_CURVE('',#3744,#3748,#2232,.T.) ;
#4701 = EDGE_CURVE('',#3748,#3748,#3218,.T.) ;
#4702 = EDGE_CURVE('',#3745,#3749,#2233,.T.) ;
#4703 = EDGE_CURVE('',#3749,#3749,#3219,.T.) ;
#4704 = EDGE_CURVE('',#3750,#3751,#2234,.T.) ;
#4705 = EDGE_CURVE('',#3752,#3750,#3220,.T.) ;
#4706 = EDGE_CURVE('',#3753,#3752,#2235,.T.) ;
#4707 = EDGE_CURVE('',#3751,#3753,#3221,.T.) ;
#4708 = EDGE_CURVE('',#3754,#3755,#2236,.T.) ;
#4709 = EDGE_CURVE('',#3756,#3754,#3222,.T.) ;
#4710 = EDGE_CURVE('',#3757,#3756,#2237,.T.) ;
#4711 = EDGE_CURVE('',#3755,#3757,#3223,.T.) ;
#4712 = EDGE_CURVE('',#3758,#3759,#2238,.T.) ;
#4713 = EDGE_CURVE('',#3760,#3758,#3224,.T.) ;
#4714 = EDGE_CURVE('',#3761,#3760,#2239,.T.) ;
#4715 = EDGE_CURVE('',#3759,#3761,#3225,.T.) ;
#4716 = EDGE_CURVE('',#3762,#3763,#2240,.T.) ;
#4717 = EDGE_CURVE('',#3764,#3762,#3226,.T.) ;
#4718 = EDGE_CURVE('',#3765,#3764,#2241,.T.) ;
#4719 = EDGE_CURVE('',#3763,#3765,#3227,.T.) ;
#4720 = EDGE_CURVE('',#3766,#3766,#3228,.T.) ;
#4721 = EDGE_CURVE('',#3764,#3753,#3229,.T.) ;
#4722 = EDGE_CURVE('',#3760,#3762,#3230,.T.) ;
#4723 = EDGE_CURVE('',#3755,#3758,#3231,.T.) ;
#4724 = EDGE_CURVE('',#3751,#3757,#3232,.T.) ;
#4725 = EDGE_CURVE('',#3761,#3763,#3233,.T.) ;
#4726 = EDGE_CURVE('',#3754,#3759,#3234,.T.) ;
#4727 = EDGE_CURVE('',#3765,#3752,#3235,.T.) ;
#4728 = EDGE_CURVE('',#3750,#3756,#3236,.T.) ;
#4729 = EDGE_CURVE('',#3767,#3767,#3237,.T.) ;
#4730 = EDGE_CURVE('',#3714,#3728,#2242,.T.) ;
#4731 = EDGE_CURVE('',#3768,#3768,#3238,.T.) ;
#4732 = EDGE_CURVE('',#3769,#3769,#3239,.T.) ;
#4733 = EDGE_CURVE('',#3768,#3770,#2243,.T.) ;
#4734 = EDGE_CURVE('',#3770,#3770,#3240,.T.) ;
#4735 = EDGE_CURVE('',#3771,#3771,#3241,.T.) ;
#4736 = EDGE_CURVE('',#3772,#3772,#3242,.T.) ;
#4737 = EDGE_CURVE('',#3772,#3771,#2244,.T.) ;
#4738 = EDGE_CURVE('',#3773,#3773,#3243,.T.) ;
#4739 = EDGE_CURVE('',#3774,#3774,#3244,.T.) ;
#4740 = EDGE_CURVE('',#3773,#3775,#2245,.T.) ;
#4741 = EDGE_CURVE('',#3775,#3775,#3245,.T.) ;
#4742 = EDGE_CURVE('',#3776,#3776,#3246,.T.) ;
#4743 = EDGE_CURVE('',#3777,#3777,#3247,.T.) ;
#4744 = EDGE_CURVE('',#3777,#3776,#2246,.T.) ;
#4745 = EDGE_CURVE('',#3774,#3778,#2247,.T.) ;
#4746 = EDGE_CURVE('',#3778,#3778,#3248,.T.) ;
#4747 = EDGE_CURVE('',#3779,#3779,#3249,.T.) ;
#4748 = EDGE_CURVE('',#3780,#3780,#3250,.T.) ;
#4749 = EDGE_CURVE('',#3780,#3779,#2248,.T.) ;
#4750 = EDGE_CURVE('',#3781,#3781,#3251,.T.) ;
#4751 = EDGE_CURVE('',#3781,#3780,#2249,.T.) ;
#4752 = EDGE_CURVE('',#3767,#3781,#2250,.T.) ;
#4753 = EDGE_CURVE('',#3782,#3782,#3252,.T.) ;
#4754 = EDGE_CURVE('',#3782,#3530,#2251,.T.) ;
#4755 = EDGE_CURVE('',#3769,#3766,#2252,.T.) ;
#4756 = EDGE_CURVE('',#3783,#3784,#2253,.T.) ;
#4757 = EDGE_CURVE('',#3783,#3785,#2254,.T.) ;
#4758 = EDGE_CURVE('',#3786,#3785,#2255,.T.) ;
#4759 = EDGE_CURVE('',#3786,#3784,#2256,.T.) ;
#4760 = EDGE_CURVE('',#3784,#3787,#3253,.T.) ;
#4761 = EDGE_CURVE('',#3788,#3786,#3254,.T.) ;
#4762 = EDGE_CURVE('',#3787,#3788,#2257,.T.) ;
#4763 = EDGE_CURVE('',#3787,#3789,#2258,.T.) ;
#4764 = EDGE_CURVE('',#3790,#3788,#2259,.T.) ;
#4765 = EDGE_CURVE('',#3790,#3789,#2260,.T.) ;
#4766 = EDGE_CURVE('',#3789,#3783,#3255,.T.) ;
#4767 = EDGE_CURVE('',#3785,#3790,#3256,.T.) ;
#4768 = EDGE_CURVE('',#3791,#3792,#2261,.T.) ;
#4769 = EDGE_CURVE('',#3791,#3793,#2262,.T.) ;
#4770 = EDGE_CURVE('',#3794,#3793,#2263,.T.) ;
#4771 = EDGE_CURVE('',#3794,#3792,#2264,.T.) ;
#4772 = EDGE_CURVE('',#3792,#3795,#3257,.T.) ;
#4773 = EDGE_CURVE('',#3796,#3794,#3258,.T.) ;
#4774 = EDGE_CURVE('',#3795,#3796,#2265,.T.) ;
#4775 = EDGE_CURVE('',#3795,#3797,#2266,.T.) ;
#4776 = EDGE_CURVE('',#3798,#3796,#2267,.T.) ;
#4777 = EDGE_CURVE('',#3798,#3797,#2268,.T.) ;
#4778 = EDGE_CURVE('',#3797,#3791,#3259,.T.) ;
#4779 = EDGE_CURVE('',#3793,#3798,#3260,.T.) ;
#4780 = EDGE_CURVE('',#3799,#3800,#2269,.T.) ;
#4781 = EDGE_CURVE('',#3799,#3801,#2270,.T.) ;
#4782 = EDGE_CURVE('',#3802,#3801,#2271,.T.) ;
#4783 = EDGE_CURVE('',#3802,#3800,#2272,.T.) ;
#4784 = EDGE_CURVE('',#3800,#3803,#3261,.T.) ;
#4785 = EDGE_CURVE('',#3804,#3802,#3262,.T.) ;
#4786 = EDGE_CURVE('',#3803,#3804,#2273,.T.) ;
#4787 = EDGE_CURVE('',#3803,#3805,#2274,.T.) ;
#4788 = EDGE_CURVE('',#3806,#3804,#2275,.T.) ;
#4789 = EDGE_CURVE('',#3806,#3805,#2276,.T.) ;
#4790 = EDGE_CURVE('',#3805,#3799,#3263,.T.) ;
#4791 = EDGE_CURVE('',#3801,#3806,#3264,.T.) ;
#4792 = EDGE_CURVE('',#3807,#3808,#2277,.T.) ;
#4793 = EDGE_CURVE('',#3807,#3809,#2278,.T.) ;
#4794 = EDGE_CURVE('',#3810,#3809,#2279,.T.) ;
#4795 = EDGE_CURVE('',#3810,#3808,#2280,.T.) ;
#4796 = EDGE_CURVE('',#3808,#3811,#3265,.T.) ;
#4797 = EDGE_CURVE('',#3812,#3810,#3266,.T.) ;
#4798 = EDGE_CURVE('',#3811,#3812,#2281,.T.) ;
#4799 = EDGE_CURVE('',#3811,#3813,#2282,.T.) ;
#4800 = EDGE_CURVE('',#3814,#3812,#2283,.T.) ;
#4801 = EDGE_CURVE('',#3814,#3813,#2284,.T.) ;
#4802 = EDGE_CURVE('',#3813,#3807,#3267,.T.) ;
#4803 = EDGE_CURVE('',#3809,#3814,#3268,.T.) ;
#4804 = EDGE_CURVE('',#3815,#3815,#3269,.T.) ;
#4805 = EDGE_CURVE('',#3815,#3816,#2285,.T.) ;
#4806 = EDGE_CURVE('',#3816,#3816,#3270,.T.) ;
#4807 = EDGE_CURVE('',#3817,#3817,#3271,.T.) ;
#4808 = EDGE_CURVE('',#3818,#3818,#3272,.T.) ;
#4809 = EDGE_CURVE('',#3818,#3817,#2286,.T.) ;
#4810 = EDGE_CURVE('',#3819,#3820,#3273,.T.) ;
#4811 = EDGE_CURVE('',#3821,#3822,#2287,.T.) ;
#4812 = EDGE_CURVE('',#3821,#3823,#625,.T.) ;
#4813 = EDGE_CURVE('',#3824,#3823,#3274,.T.) ;
#4814 = EDGE_CURVE('',#3824,#3822,#626,.T.) ;
#4815 = EDGE_CURVE('',#3825,#3826,#2288,.T.) ;
#4816 = EDGE_CURVE('',#3825,#3821,#627,.T.) ;
#4817 = EDGE_CURVE('',#3822,#3826,#628,.T.) ;
#4818 = EDGE_CURVE('',#3827,#3828,#2289,.T.) ;
#4819 = EDGE_CURVE('',#3827,#3825,#629,.T.) ;
#4820 = EDGE_CURVE('',#3826,#3828,#630,.T.) ;
#4821 = EDGE_CURVE('',#3829,#3830,#2290,.T.) ;
#4822 = EDGE_CURVE('',#3829,#3827,#631,.T.) ;
#4823 = EDGE_CURVE('',#3828,#3830,#632,.T.) ;
#4824 = EDGE_CURVE('',#3831,#3832,#2291,.T.) ;
#4825 = EDGE_CURVE('',#3831,#3829,#633,.T.) ;
#4826 = EDGE_CURVE('',#3830,#3832,#634,.T.) ;
#4827 = EDGE_CURVE('',#3833,#3834,#2292,.T.) ;
#4828 = EDGE_CURVE('',#3833,#3831,#635,.T.) ;
#4829 = EDGE_CURVE('',#3832,#3834,#636,.T.) ;
#4830 = EDGE_CURVE('',#3835,#3836,#2293,.T.) ;
#4831 = EDGE_CURVE('',#3835,#3833,#637,.T.) ;
#4832 = EDGE_CURVE('',#3834,#3836,#638,.T.) ;
#4833 = EDGE_CURVE('',#3837,#3838,#2294,.T.) ;
#4834 = EDGE_CURVE('',#3837,#3835,#639,.T.) ;
#4835 = EDGE_CURVE('',#3836,#3838,#640,.T.) ;
#4836 = EDGE_CURVE('',#3839,#3840,#2295,.T.) ;
#4837 = EDGE_CURVE('',#3839,#3837,#641,.T.) ;
#4838 = EDGE_CURVE('',#3838,#3840,#642,.T.) ;
#4839 = EDGE_CURVE('',#3841,#3842,#2296,.T.) ;
#4840 = EDGE_CURVE('',#3841,#3839,#643,.T.) ;
#4841 = EDGE_CURVE('',#3840,#3842,#644,.T.) ;
#4842 = EDGE_CURVE('',#3843,#3844,#2297,.T.) ;
#4843 = EDGE_CURVE('',#3843,#3841,#645,.T.) ;
#4844 = EDGE_CURVE('',#3842,#3844,#646,.T.) ;
#4845 = EDGE_CURVE('',#3845,#3846,#2298,.T.) ;
#4846 = EDGE_CURVE('',#3845,#3843,#647,.T.) ;
#4847 = EDGE_CURVE('',#3844,#3846,#648,.T.) ;
#4848 = EDGE_CURVE('',#3847,#3848,#2299,.T.) ;
#4849 = EDGE_CURVE('',#3847,#3845,#649,.T.) ;
#4850 = EDGE_CURVE('',#3846,#3848,#650,.T.) ;
#4851 = EDGE_CURVE('',#3849,#3850,#2300,.T.) ;
#4852 = EDGE_CURVE('',#3851,#3849,#3275,.T.) ;
#4853 = EDGE_CURVE('',#3851,#3847,#651,.T.) ;
#4854 = EDGE_CURVE('',#3848,#3850,#652,.T.) ;
#4855 = EDGE_CURVE('',#3852,#3853,#2301,.T.) ;
#4856 = EDGE_CURVE('',#3852,#3854,#653,.T.) ;
#4857 = EDGE_CURVE('',#3855,#3854,#3276,.T.) ;
#4858 = EDGE_CURVE('',#3853,#3855,#654,.T.) ;
#4859 = EDGE_CURVE('',#3856,#3857,#2302,.T.) ;
#4860 = EDGE_CURVE('',#3856,#3852,#655,.T.) ;
#4861 = EDGE_CURVE('',#3857,#3853,#656,.T.) ;
#4862 = EDGE_CURVE('',#3858,#3859,#2303,.T.) ;
#4863 = EDGE_CURVE('',#3858,#3856,#657,.T.) ;
#4864 = EDGE_CURVE('',#3859,#3857,#658,.T.) ;
#4865 = EDGE_CURVE('',#3860,#3861,#2304,.T.) ;
#4866 = EDGE_CURVE('',#3860,#3858,#659,.T.) ;
#4867 = EDGE_CURVE('',#3861,#3859,#660,.T.) ;
#4868 = EDGE_CURVE('',#3862,#3863,#2305,.T.) ;
#4869 = EDGE_CURVE('',#3862,#3860,#661,.T.) ;
#4870 = EDGE_CURVE('',#3863,#3861,#662,.T.) ;
#4871 = EDGE_CURVE('',#3864,#3865,#2306,.T.) ;
#4872 = EDGE_CURVE('',#3864,#3862,#663,.T.) ;
#4873 = EDGE_CURVE('',#3865,#3863,#664,.T.) ;
#4874 = EDGE_CURVE('',#3866,#3867,#2307,.T.) ;
#4875 = EDGE_CURVE('',#3866,#3864,#665,.T.) ;
#4876 = EDGE_CURVE('',#3867,#3865,#666,.T.) ;
#4877 = EDGE_CURVE('',#3868,#3869,#2308,.T.) ;
#4878 = EDGE_CURVE('',#3868,#3866,#667,.T.) ;
#4879 = EDGE_CURVE('',#3869,#3867,#668,.T.) ;
#4880 = EDGE_CURVE('',#3870,#3871,#2309,.T.) ;
#4881 = EDGE_CURVE('',#3870,#3868,#669,.T.) ;
#4882 = EDGE_CURVE('',#3871,#3869,#670,.T.) ;
#4883 = EDGE_CURVE('',#3872,#3873,#2310,.T.) ;
#4884 = EDGE_CURVE('',#3872,#3870,#671,.T.) ;
#4885 = EDGE_CURVE('',#3873,#3871,#672,.T.) ;
#4886 = EDGE_CURVE('',#3874,#3875,#2311,.T.) ;
#4887 = EDGE_CURVE('',#3874,#3872,#673,.T.) ;
#4888 = EDGE_CURVE('',#3875,#3873,#674,.T.) ;
#4889 = EDGE_CURVE('',#3876,#3877,#2312,.T.) ;
#4890 = EDGE_CURVE('',#3876,#3874,#675,.T.) ;
#4891 = EDGE_CURVE('',#3877,#3875,#676,.T.) ;
#4892 = EDGE_CURVE('',#3878,#3879,#2313,.T.) ;
#4893 = EDGE_CURVE('',#3878,#3876,#677,.T.) ;
#4894 = EDGE_CURVE('',#3879,#3877,#678,.T.) ;
#4895 = EDGE_CURVE('',#3854,#3851,#679,.T.) ;
#4896 = EDGE_CURVE('',#3880,#3851,#3277,.T.) ;
#4897 = EDGE_CURVE('',#3880,#3855,#680,.T.) ;
#4898 = EDGE_CURVE('',#3850,#3880,#681,.T.) ;
#4899 = EDGE_CURVE('',#3881,#3824,#682,.T.) ;
#4900 = EDGE_CURVE('',#3881,#3879,#683,.T.) ;
#4901 = EDGE_CURVE('',#3823,#3882,#3278,.T.) ;
#4902 = EDGE_CURVE('',#3823,#3883,#684,.T.) ;
#4903 = EDGE_CURVE('',#3883,#3881,#3279,.T.) ;
#4904 = EDGE_CURVE('',#3882,#3824,#3280,.T.) ;
#4905 = EDGE_CURVE('',#3883,#3878,#685,.T.) ;
#4906 = EDGE_CURVE('',#3882,#3884,#3281,.T.) ;
#4907 = EDGE_CURVE('',#3884,#3884,#3282,.T.) ;
#4908 = EDGE_CURVE('',#3849,#3880,#3283,.T.) ;
#4909 = EDGE_CURVE('',#3885,#3885,#3284,.T.) ;
#4910 = EDGE_CURVE('',#3849,#3886,#2314,.T.) ;
#4911 = EDGE_CURVE('',#3886,#3886,#3285,.T.) ;
#4912 = EDGE_CURVE('',#3887,#3888,#231,.T.) ;
#4913 = EDGE_CURVE('',#3887,#3889,#2315,.T.) ;
#4914 = EDGE_CURVE('',#3889,#3890,#2316,.T.) ;
#4915 = EDGE_CURVE('',#3888,#3890,#2317,.T.) ;
#4916 = EDGE_CURVE('',#3890,#3891,#3286,.T.) ;
#4917 = EDGE_CURVE('',#3891,#3889,#2318,.T.) ;
#4918 = EDGE_CURVE('',#3892,#3887,#232,.T.) ;
#4919 = EDGE_CURVE('',#3891,#3892,#2319,.T.) ;
#4920 = EDGE_CURVE('',#3893,#3892,#3287,.T.) ;
#4921 = EDGE_CURVE('',#3893,#3894,#2320,.T.) ;
#4922 = EDGE_CURVE('',#3894,#3895,#3288,.T.) ;
#4923 = EDGE_CURVE('',#3895,#3896,#2321,.T.) ;
#4924 = EDGE_CURVE('',#3897,#3896,#3289,.T.) ;
#4925 = EDGE_CURVE('',#3897,#3898,#2322,.T.) ;
#4926 = EDGE_CURVE('',#3898,#3899,#3290,.T.) ;
#4927 = EDGE_CURVE('',#3899,#3900,#2323,.T.) ;
#4928 = EDGE_CURVE('',#3901,#3900,#3291,.T.) ;
#4929 = EDGE_CURVE('',#3901,#3902,#2324,.T.) ;
#4930 = EDGE_CURVE('',#3902,#3903,#3292,.T.) ;
#4931 = EDGE_CURVE('',#3903,#3904,#2325,.T.) ;
#4932 = EDGE_CURVE('',#3905,#3904,#3293,.T.) ;
#4933 = EDGE_CURVE('',#3905,#3906,#2326,.T.) ;
#4934 = EDGE_CURVE('',#3906,#3907,#3294,.T.) ;
#4935 = EDGE_CURVE('',#3907,#3908,#2327,.T.) ;
#4936 = EDGE_CURVE('',#3909,#3908,#3295,.T.) ;
#4937 = EDGE_CURVE('',#3909,#3910,#2328,.T.) ;
#4938 = EDGE_CURVE('',#3910,#3911,#3296,.T.) ;
#4939 = EDGE_CURVE('',#3911,#3912,#2329,.T.) ;
#4940 = EDGE_CURVE('',#3913,#3912,#3297,.T.) ;
#4941 = EDGE_CURVE('',#3913,#3914,#2330,.T.) ;
#4942 = EDGE_CURVE('',#3914,#3915,#3298,.T.) ;
#4943 = EDGE_CURVE('',#3915,#3916,#2331,.T.) ;
#4944 = EDGE_CURVE('',#3917,#3916,#3299,.T.) ;
#4945 = EDGE_CURVE('',#3917,#3918,#2332,.T.) ;
#4946 = EDGE_CURVE('',#3918,#3919,#3300,.T.) ;
#4947 = EDGE_CURVE('',#3919,#3920,#2333,.T.) ;
#4948 = EDGE_CURVE('',#3921,#3920,#3301,.T.) ;
#4949 = EDGE_CURVE('',#3921,#3922,#2334,.T.) ;
#4950 = EDGE_CURVE('',#3922,#3923,#3302,.T.) ;
#4951 = EDGE_CURVE('',#3923,#3924,#2335,.T.) ;
#4952 = EDGE_CURVE('',#3925,#3924,#3303,.T.) ;
#4953 = EDGE_CURVE('',#3925,#3926,#2336,.T.) ;
#4954 = EDGE_CURVE('',#3926,#3927,#3304,.T.) ;
#4955 = EDGE_CURVE('',#3927,#3928,#2337,.T.) ;
#4956 = EDGE_CURVE('',#3929,#3928,#3305,.T.) ;
#4957 = EDGE_CURVE('',#3929,#3930,#2338,.T.) ;
#4958 = EDGE_CURVE('',#3930,#3931,#3306,.T.) ;
#4959 = EDGE_CURVE('',#3931,#3932,#2339,.T.) ;
#4960 = EDGE_CURVE('',#3933,#3932,#3307,.T.) ;
#4961 = EDGE_CURVE('',#3933,#3934,#2340,.T.) ;
#4962 = EDGE_CURVE('',#3934,#3935,#3308,.T.) ;
#4963 = EDGE_CURVE('',#3935,#3936,#2341,.T.) ;
#4964 = EDGE_CURVE('',#3937,#3936,#3309,.T.) ;
#4965 = EDGE_CURVE('',#3937,#3938,#2342,.T.) ;
#4966 = EDGE_CURVE('',#3938,#3939,#3310,.T.) ;
#4967 = EDGE_CURVE('',#3939,#3940,#2343,.T.) ;
#4968 = EDGE_CURVE('',#3941,#3940,#3311,.T.) ;
#4969 = EDGE_CURVE('',#3941,#3942,#2344,.T.) ;
#4970 = EDGE_CURVE('',#3942,#3943,#3312,.T.) ;
#4971 = EDGE_CURVE('',#3943,#3944,#2345,.T.) ;
#4972 = EDGE_CURVE('',#3945,#3944,#3313,.T.) ;
#4973 = EDGE_CURVE('',#3945,#3946,#2346,.T.) ;
#4974 = EDGE_CURVE('',#3946,#3947,#3314,.T.) ;
#4975 = EDGE_CURVE('',#3947,#3948,#2347,.T.) ;
#4976 = EDGE_CURVE('',#3949,#3948,#3315,.T.) ;
#4977 = EDGE_CURVE('',#3949,#3950,#2348,.T.) ;
#4978 = EDGE_CURVE('',#3950,#3951,#3316,.T.) ;
#4979 = EDGE_CURVE('',#3951,#3952,#2349,.T.) ;
#4980 = EDGE_CURVE('',#3953,#3952,#3317,.T.) ;
#4981 = EDGE_CURVE('',#3953,#3954,#2350,.T.) ;
#4982 = EDGE_CURVE('',#3954,#3955,#3318,.T.) ;
#4983 = EDGE_CURVE('',#3955,#3956,#2351,.T.) ;
#4984 = EDGE_CURVE('',#3957,#3956,#3319,.T.) ;
#4985 = EDGE_CURVE('',#3957,#3958,#2352,.T.) ;
#4986 = EDGE_CURVE('',#3958,#3959,#3320,.T.) ;
#4987 = EDGE_CURVE('',#3959,#3960,#2353,.T.) ;
#4988 = EDGE_CURVE('',#3961,#3960,#3321,.T.) ;
#4989 = EDGE_CURVE('',#3961,#3962,#2354,.T.) ;
#4990 = EDGE_CURVE('',#3962,#3963,#3322,.T.) ;
#4991 = EDGE_CURVE('',#3963,#3964,#2355,.T.) ;
#4992 = EDGE_CURVE('',#3965,#3964,#3323,.T.) ;
#4993 = EDGE_CURVE('',#3965,#3966,#2356,.T.) ;
#4994 = EDGE_CURVE('',#3966,#3967,#3324,.T.) ;
#4995 = EDGE_CURVE('',#3967,#3968,#2357,.T.) ;
#4996 = EDGE_CURVE('',#3969,#3968,#3325,.T.) ;
#4997 = EDGE_CURVE('',#3969,#3970,#2358,.T.) ;
#4998 = EDGE_CURVE('',#3970,#3971,#3326,.T.) ;
#4999 = EDGE_CURVE('',#3971,#3972,#2359,.T.) ;
#5000 = EDGE_CURVE('',#3973,#3972,#3327,.T.) ;
#5001 = EDGE_CURVE('',#3973,#3974,#2360,.T.) ;
#5002 = EDGE_CURVE('',#3974,#3975,#3328,.T.) ;
#5003 = EDGE_CURVE('',#3975,#3976,#2361,.T.) ;
#5004 = EDGE_CURVE('',#3977,#3976,#3329,.T.) ;
#5005 = EDGE_CURVE('',#3977,#3978,#2362,.T.) ;
#5006 = EDGE_CURVE('',#3978,#3979,#3330,.T.) ;
#5007 = EDGE_CURVE('',#3979,#3980,#2363,.T.) ;
#5008 = EDGE_CURVE('',#3981,#3980,#3331,.T.) ;
#5009 = EDGE_CURVE('',#3981,#3982,#2364,.T.) ;
#5010 = EDGE_CURVE('',#3982,#3983,#3332,.T.) ;
#5011 = EDGE_CURVE('',#3983,#3984,#2365,.T.) ;
#5012 = EDGE_CURVE('',#3985,#3984,#3333,.T.) ;
#5013 = EDGE_CURVE('',#3985,#3986,#2366,.T.) ;
#5014 = EDGE_CURVE('',#3986,#3987,#3334,.T.) ;
#5015 = EDGE_CURVE('',#3987,#3988,#2367,.T.) ;
#5016 = EDGE_CURVE('',#3989,#3988,#3335,.T.) ;
#5017 = EDGE_CURVE('',#3989,#3990,#2368,.T.) ;
#5018 = EDGE_CURVE('',#3990,#3991,#3336,.T.) ;
#5019 = EDGE_CURVE('',#3991,#3992,#2369,.T.) ;
#5020 = EDGE_CURVE('',#3993,#3992,#3337,.T.) ;
#5021 = EDGE_CURVE('',#3993,#3994,#2370,.T.) ;
#5022 = EDGE_CURVE('',#3994,#3995,#3338,.T.) ;
#5023 = EDGE_CURVE('',#3995,#3996,#2371,.T.) ;
#5024 = EDGE_CURVE('',#3997,#3996,#3339,.T.) ;
#5025 = EDGE_CURVE('',#3997,#3998,#2372,.T.) ;
#5026 = EDGE_CURVE('',#3998,#3999,#3340,.T.) ;
#5027 = EDGE_CURVE('',#3999,#4000,#2373,.T.) ;
#5028 = EDGE_CURVE('',#4001,#4000,#3341,.T.) ;
#5029 = EDGE_CURVE('',#4001,#4002,#2374,.T.) ;
#5030 = EDGE_CURVE('',#4002,#4003,#3342,.T.) ;
#5031 = EDGE_CURVE('',#4003,#4004,#2375,.T.) ;
#5032 = EDGE_CURVE('',#4004,#4004,#3343,.T.) ;
#5033 = EDGE_CURVE('',#4003,#4005,#3344,.T.) ;
#5034 = EDGE_CURVE('',#4005,#4006,#2376,.T.) ;
#5035 = EDGE_CURVE('',#4007,#4006,#3345,.T.) ;
#5036 = EDGE_CURVE('',#4007,#4008,#2377,.T.) ;
#5037 = EDGE_CURVE('',#4008,#4009,#3346,.T.) ;
#5038 = EDGE_CURVE('',#4009,#4010,#2378,.T.) ;
#5039 = EDGE_CURVE('',#4011,#4010,#3347,.T.) ;
#5040 = EDGE_CURVE('',#4011,#4012,#2379,.T.) ;
#5041 = EDGE_CURVE('',#4012,#4013,#3348,.T.) ;
#5042 = EDGE_CURVE('',#4013,#4014,#2380,.T.) ;
#5043 = EDGE_CURVE('',#4015,#4014,#3349,.T.) ;
#5044 = EDGE_CURVE('',#4015,#4016,#2381,.T.) ;
#5045 = EDGE_CURVE('',#4016,#4017,#3350,.T.) ;
#5046 = EDGE_CURVE('',#4017,#4018,#2382,.T.) ;
#5047 = EDGE_CURVE('',#4019,#4018,#3351,.T.) ;
#5048 = EDGE_CURVE('',#4019,#4020,#2383,.T.) ;
#5049 = EDGE_CURVE('',#4020,#4021,#3352,.T.) ;
#5050 = EDGE_CURVE('',#4021,#4022,#2384,.T.) ;
#5051 = EDGE_CURVE('',#4023,#4022,#3353,.T.) ;
#5052 = EDGE_CURVE('',#4023,#4024,#2385,.T.) ;
#5053 = EDGE_CURVE('',#4024,#4025,#3354,.T.) ;
#5054 = EDGE_CURVE('',#4025,#4026,#2386,.T.) ;
#5055 = EDGE_CURVE('',#4027,#4026,#3355,.T.) ;
#5056 = EDGE_CURVE('',#4027,#4028,#2387,.T.) ;
#5057 = EDGE_CURVE('',#4028,#4029,#3356,.T.) ;
#5058 = EDGE_CURVE('',#4029,#4030,#2388,.T.) ;
#5059 = EDGE_CURVE('',#4031,#4030,#3357,.T.) ;
#5060 = EDGE_CURVE('',#4031,#4032,#2389,.T.) ;
#5061 = EDGE_CURVE('',#4032,#4033,#3358,.T.) ;
#5062 = EDGE_CURVE('',#4033,#4034,#2390,.T.) ;
#5063 = EDGE_CURVE('',#3888,#4034,#3359,.T.) ;
#5064 = EDGE_CURVE('',#4035,#4031,#233,.T.) ;
#5065 = EDGE_CURVE('',#4035,#4036,#2391,.T.) ;
#5066 = EDGE_CURVE('',#4036,#4032,#2392,.T.) ;
#5067 = EDGE_CURVE('',#4033,#4036,#2393,.T.) ;
#5068 = EDGE_CURVE('',#4034,#4035,#234,.T.) ;
#5069 = EDGE_CURVE('',#4037,#4027,#235,.T.) ;
#5070 = EDGE_CURVE('',#4037,#4038,#2394,.T.) ;
#5071 = EDGE_CURVE('',#4038,#4028,#2395,.T.) ;
#5072 = EDGE_CURVE('',#4029,#4038,#2396,.T.) ;
#5073 = EDGE_CURVE('',#4030,#4037,#236,.T.) ;
#5074 = EDGE_CURVE('',#4039,#4023,#237,.T.) ;
#5075 = EDGE_CURVE('',#4039,#4040,#2397,.T.) ;
#5076 = EDGE_CURVE('',#4040,#4024,#2398,.T.) ;
#5077 = EDGE_CURVE('',#4025,#4040,#2399,.T.) ;
#5078 = EDGE_CURVE('',#4026,#4039,#238,.T.) ;
#5079 = EDGE_CURVE('',#4041,#4019,#239,.T.) ;
#5080 = EDGE_CURVE('',#4041,#4042,#2400,.T.) ;
#5081 = EDGE_CURVE('',#4042,#4020,#2401,.T.) ;
#5082 = EDGE_CURVE('',#4021,#4042,#2402,.T.) ;
#5083 = EDGE_CURVE('',#4022,#4041,#240,.T.) ;
#5084 = EDGE_CURVE('',#4043,#4015,#241,.T.) ;
#5085 = EDGE_CURVE('',#4043,#4044,#2403,.T.) ;
#5086 = EDGE_CURVE('',#4044,#4016,#2404,.T.) ;
#5087 = EDGE_CURVE('',#4017,#4044,#2405,.T.) ;
#5088 = EDGE_CURVE('',#4018,#4043,#242,.T.) ;
#5089 = EDGE_CURVE('',#4045,#4011,#243,.T.) ;
#5090 = EDGE_CURVE('',#4045,#4046,#2406,.T.) ;
#5091 = EDGE_CURVE('',#4046,#4012,#2407,.T.) ;
#5092 = EDGE_CURVE('',#4013,#4046,#2408,.T.) ;
#5093 = EDGE_CURVE('',#4014,#4045,#244,.T.) ;
#5094 = EDGE_CURVE('',#4047,#4007,#245,.T.) ;
#5095 = EDGE_CURVE('',#4047,#4048,#2409,.T.) ;
#5096 = EDGE_CURVE('',#4048,#4008,#2410,.T.) ;
#5097 = EDGE_CURVE('',#4009,#4048,#2411,.T.) ;
#5098 = EDGE_CURVE('',#4010,#4047,#246,.T.) ;
#5099 = EDGE_CURVE('',#4049,#4001,#247,.T.) ;
#5100 = EDGE_CURVE('',#4049,#4050,#2412,.T.) ;
#5101 = EDGE_CURVE('',#4050,#4002,#2413,.T.) ;
#5102 = EDGE_CURVE('',#4005,#4050,#2414,.T.) ;
#5103 = EDGE_CURVE('',#4006,#4049,#248,.T.) ;
#5104 = EDGE_CURVE('',#4051,#3997,#249,.T.) ;
#5105 = EDGE_CURVE('',#4051,#4052,#2415,.T.) ;
#5106 = EDGE_CURVE('',#4052,#3998,#2416,.T.) ;
#5107 = EDGE_CURVE('',#3999,#4052,#2417,.T.) ;
#5108 = EDGE_CURVE('',#4000,#4051,#250,.T.) ;
#5109 = EDGE_CURVE('',#4053,#3993,#251,.T.) ;
#5110 = EDGE_CURVE('',#4053,#4054,#2418,.T.) ;
#5111 = EDGE_CURVE('',#4054,#3994,#2419,.T.) ;
#5112 = EDGE_CURVE('',#3995,#4054,#2420,.T.) ;
#5113 = EDGE_CURVE('',#3996,#4053,#252,.T.) ;
#5114 = EDGE_CURVE('',#4055,#3989,#253,.T.) ;
#5115 = EDGE_CURVE('',#4055,#4056,#2421,.T.) ;
#5116 = EDGE_CURVE('',#4056,#3990,#2422,.T.) ;
#5117 = EDGE_CURVE('',#3991,#4056,#2423,.T.) ;
#5118 = EDGE_CURVE('',#3992,#4055,#254,.T.) ;
#5119 = EDGE_CURVE('',#4057,#3985,#255,.T.) ;
#5120 = EDGE_CURVE('',#4057,#4058,#2424,.T.) ;
#5121 = EDGE_CURVE('',#4058,#3986,#2425,.T.) ;
#5122 = EDGE_CURVE('',#3987,#4058,#2426,.T.) ;
#5123 = EDGE_CURVE('',#3988,#4057,#256,.T.) ;
#5124 = EDGE_CURVE('',#4059,#3981,#257,.T.) ;
#5125 = EDGE_CURVE('',#4059,#4060,#2427,.T.) ;
#5126 = EDGE_CURVE('',#4060,#3982,#2428,.T.) ;
#5127 = EDGE_CURVE('',#3983,#4060,#2429,.T.) ;
#5128 = EDGE_CURVE('',#3984,#4059,#258,.T.) ;
#5129 = EDGE_CURVE('',#4061,#3977,#259,.T.) ;
#5130 = EDGE_CURVE('',#4061,#4062,#2430,.T.) ;
#5131 = EDGE_CURVE('',#4062,#3978,#2431,.T.) ;
#5132 = EDGE_CURVE('',#3979,#4062,#2432,.T.) ;
#5133 = EDGE_CURVE('',#3980,#4061,#260,.T.) ;
#5134 = EDGE_CURVE('',#4063,#3973,#261,.T.) ;
#5135 = EDGE_CURVE('',#4063,#4064,#2433,.T.) ;
#5136 = EDGE_CURVE('',#4064,#3974,#2434,.T.) ;
#5137 = EDGE_CURVE('',#3975,#4064,#2435,.T.) ;
#5138 = EDGE_CURVE('',#3976,#4063,#262,.T.) ;
#5139 = EDGE_CURVE('',#4065,#3969,#263,.T.) ;
#5140 = EDGE_CURVE('',#4065,#4066,#2436,.T.) ;
#5141 = EDGE_CURVE('',#4066,#3970,#2437,.T.) ;
#5142 = EDGE_CURVE('',#3971,#4066,#2438,.T.) ;
#5143 = EDGE_CURVE('',#3972,#4065,#264,.T.) ;
#5144 = EDGE_CURVE('',#4067,#3965,#265,.T.) ;
#5145 = EDGE_CURVE('',#4067,#4068,#2439,.T.) ;
#5146 = EDGE_CURVE('',#4068,#3966,#2440,.T.) ;
#5147 = EDGE_CURVE('',#3967,#4068,#2441,.T.) ;
#5148 = EDGE_CURVE('',#3968,#4067,#266,.T.) ;
#5149 = EDGE_CURVE('',#4069,#3961,#267,.T.) ;
#5150 = EDGE_CURVE('',#4069,#4070,#2442,.T.) ;
#5151 = EDGE_CURVE('',#4070,#3962,#2443,.T.) ;
#5152 = EDGE_CURVE('',#3963,#4070,#2444,.T.) ;
#5153 = EDGE_CURVE('',#3964,#4069,#268,.T.) ;
#5154 = EDGE_CURVE('',#4071,#3957,#269,.T.) ;
#5155 = EDGE_CURVE('',#4071,#4072,#2445,.T.) ;
#5156 = EDGE_CURVE('',#4072,#3958,#2446,.T.) ;
#5157 = EDGE_CURVE('',#3959,#4072,#2447,.T.) ;
#5158 = EDGE_CURVE('',#3960,#4071,#270,.T.) ;
#5159 = EDGE_CURVE('',#4073,#3953,#271,.T.) ;
#5160 = EDGE_CURVE('',#4073,#4074,#2448,.T.) ;
#5161 = EDGE_CURVE('',#4074,#3954,#2449,.T.) ;
#5162 = EDGE_CURVE('',#3955,#4074,#2450,.T.) ;
#5163 = EDGE_CURVE('',#3956,#4073,#272,.T.) ;
#5164 = EDGE_CURVE('',#4075,#3949,#273,.T.) ;
#5165 = EDGE_CURVE('',#4075,#4076,#2451,.T.) ;
#5166 = EDGE_CURVE('',#4076,#3950,#2452,.T.) ;
#5167 = EDGE_CURVE('',#3951,#4076,#2453,.T.) ;
#5168 = EDGE_CURVE('',#3952,#4075,#274,.T.) ;
#5169 = EDGE_CURVE('',#4077,#3945,#275,.T.) ;
#5170 = EDGE_CURVE('',#4077,#4078,#2454,.T.) ;
#5171 = EDGE_CURVE('',#4078,#3946,#2455,.T.) ;
#5172 = EDGE_CURVE('',#3947,#4078,#2456,.T.) ;
#5173 = EDGE_CURVE('',#3948,#4077,#276,.T.) ;
#5174 = EDGE_CURVE('',#4079,#3941,#277,.T.) ;
#5175 = EDGE_CURVE('',#4079,#4080,#2457,.T.) ;
#5176 = EDGE_CURVE('',#4080,#3942,#2458,.T.) ;
#5177 = EDGE_CURVE('',#3943,#4080,#2459,.T.) ;
#5178 = EDGE_CURVE('',#3944,#4079,#278,.T.) ;
#5179 = EDGE_CURVE('',#4081,#3937,#279,.T.) ;
#5180 = EDGE_CURVE('',#4081,#4082,#2460,.T.) ;
#5181 = EDGE_CURVE('',#4082,#3938,#2461,.T.) ;
#5182 = EDGE_CURVE('',#3939,#4082,#2462,.T.) ;
#5183 = EDGE_CURVE('',#3940,#4081,#280,.T.) ;
#5184 = EDGE_CURVE('',#4083,#3933,#281,.T.) ;
#5185 = EDGE_CURVE('',#4083,#4084,#2463,.T.) ;
#5186 = EDGE_CURVE('',#4084,#3934,#2464,.T.) ;
#5187 = EDGE_CURVE('',#3935,#4084,#2465,.T.) ;
#5188 = EDGE_CURVE('',#3936,#4083,#282,.T.) ;
#5189 = EDGE_CURVE('',#4085,#3929,#283,.T.) ;
#5190 = EDGE_CURVE('',#4085,#4086,#2466,.T.) ;
#5191 = EDGE_CURVE('',#4086,#3930,#2467,.T.) ;
#5192 = EDGE_CURVE('',#3931,#4086,#2468,.T.) ;
#5193 = EDGE_CURVE('',#3932,#4085,#284,.T.) ;
#5194 = EDGE_CURVE('',#4087,#3925,#285,.T.) ;
#5195 = EDGE_CURVE('',#4087,#4088,#2469,.T.) ;
#5196 = EDGE_CURVE('',#4088,#3926,#2470,.T.) ;
#5197 = EDGE_CURVE('',#3927,#4088,#2471,.T.) ;
#5198 = EDGE_CURVE('',#3928,#4087,#286,.T.) ;
#5199 = EDGE_CURVE('',#4089,#3921,#287,.T.) ;
#5200 = EDGE_CURVE('',#4089,#4090,#2472,.T.) ;
#5201 = EDGE_CURVE('',#4090,#3922,#2473,.T.) ;
#5202 = EDGE_CURVE('',#3923,#4090,#2474,.T.) ;
#5203 = EDGE_CURVE('',#3924,#4089,#288,.T.) ;
#5204 = EDGE_CURVE('',#4091,#3917,#289,.T.) ;
#5205 = EDGE_CURVE('',#4091,#4092,#2475,.T.) ;
#5206 = EDGE_CURVE('',#4092,#3918,#2476,.T.) ;
#5207 = EDGE_CURVE('',#3919,#4092,#2477,.T.) ;
#5208 = EDGE_CURVE('',#3920,#4091,#290,.T.) ;
#5209 = EDGE_CURVE('',#4093,#3913,#291,.T.) ;
#5210 = EDGE_CURVE('',#4093,#4094,#2478,.T.) ;
#5211 = EDGE_CURVE('',#4094,#3914,#2479,.T.) ;
#5212 = EDGE_CURVE('',#3915,#4094,#2480,.T.) ;
#5213 = EDGE_CURVE('',#3916,#4093,#292,.T.) ;
#5214 = EDGE_CURVE('',#4095,#3909,#293,.T.) ;
#5215 = EDGE_CURVE('',#4095,#4096,#2481,.T.) ;
#5216 = EDGE_CURVE('',#4096,#3910,#2482,.T.) ;
#5217 = EDGE_CURVE('',#3911,#4096,#2483,.T.) ;
#5218 = EDGE_CURVE('',#3912,#4095,#294,.T.) ;
#5219 = EDGE_CURVE('',#4097,#3905,#295,.T.) ;
#5220 = EDGE_CURVE('',#4097,#4098,#2484,.T.) ;
#5221 = EDGE_CURVE('',#4098,#3906,#2485,.T.) ;
#5222 = EDGE_CURVE('',#3907,#4098,#2486,.T.) ;
#5223 = EDGE_CURVE('',#3908,#4097,#296,.T.) ;
#5224 = EDGE_CURVE('',#4099,#3901,#297,.T.) ;
#5225 = EDGE_CURVE('',#4099,#4100,#2487,.T.) ;
#5226 = EDGE_CURVE('',#4100,#3902,#2488,.T.) ;
#5227 = EDGE_CURVE('',#3903,#4100,#2489,.T.) ;
#5228 = EDGE_CURVE('',#3904,#4099,#298,.T.) ;
#5229 = EDGE_CURVE('',#4101,#3897,#299,.T.) ;
#5230 = EDGE_CURVE('',#4101,#4102,#2490,.T.) ;
#5231 = EDGE_CURVE('',#4102,#3898,#2491,.T.) ;
#5232 = EDGE_CURVE('',#3899,#4102,#2492,.T.) ;
#5233 = EDGE_CURVE('',#3900,#4101,#300,.T.) ;
#5234 = EDGE_CURVE('',#4103,#3893,#301,.T.) ;
#5235 = EDGE_CURVE('',#4103,#4104,#2493,.T.) ;
#5236 = EDGE_CURVE('',#4104,#3894,#2494,.T.) ;
#5237 = EDGE_CURVE('',#3895,#4104,#2495,.T.) ;
#5238 = EDGE_CURVE('',#3896,#4103,#302,.T.) ;
#5239 = EDGE_CURVE('',#4004,#3885,#3360,.T.) ;
#5240 = EDGE_CURVE('',#4105,#4105,#3361,.T.) ;
#5241 = EDGE_CURVE('',#4105,#4049,#2496,.T.) ;
#5242 = EDGE_CURVE('',#4106,#4106,#3362,.T.) ;
#5243 = EDGE_CURVE('',#4107,#4108,#303,.T.) ;
#5244 = EDGE_CURVE('',#4109,#4107,#3363,.T.) ;
#5245 = EDGE_CURVE('',#4110,#4109,#304,.T.) ;
#5246 = EDGE_CURVE('',#4111,#4110,#305,.T.) ;
#5247 = EDGE_CURVE('',#4112,#4111,#3364,.T.) ;
#5248 = EDGE_CURVE('',#4113,#4112,#306,.T.) ;
#5249 = EDGE_CURVE('',#4114,#4113,#307,.T.) ;
#5250 = EDGE_CURVE('',#4115,#4114,#3365,.T.) ;
#5251 = EDGE_CURVE('',#4116,#4115,#308,.T.) ;
#5252 = EDGE_CURVE('',#4117,#4116,#309,.T.) ;
#5253 = EDGE_CURVE('',#4118,#4117,#3366,.T.) ;
#5254 = EDGE_CURVE('',#4119,#4118,#310,.T.) ;
#5255 = EDGE_CURVE('',#4120,#4119,#311,.T.) ;
#5256 = EDGE_CURVE('',#4121,#4120,#3367,.T.) ;
#5257 = EDGE_CURVE('',#4122,#4121,#312,.T.) ;
#5258 = EDGE_CURVE('',#4122,#4106,#2497,.T.) ;
#5259 = EDGE_CURVE('',#4123,#4122,#313,.T.) ;
#5260 = EDGE_CURVE('',#4124,#4123,#3368,.T.) ;
#5261 = EDGE_CURVE('',#4108,#4124,#314,.T.) ;
#5262 = EDGE_CURVE('',#4118,#4125,#2498,.T.) ;
#5263 = EDGE_CURVE('',#4126,#4117,#2499,.T.) ;
#5264 = EDGE_CURVE('',#4125,#4126,#3369,.T.) ;
#5265 = EDGE_CURVE('',#4127,#4114,#2500,.T.) ;
#5266 = EDGE_CURVE('',#4128,#4127,#3370,.T.) ;
#5267 = EDGE_CURVE('',#4115,#4128,#2501,.T.) ;
#5268 = EDGE_CURVE('',#4121,#4129,#2502,.T.) ;
#5269 = EDGE_CURVE('',#4130,#4120,#2503,.T.) ;
#5270 = EDGE_CURVE('',#4129,#4130,#3371,.T.) ;
#5271 = EDGE_CURVE('',#4131,#4111,#2504,.T.) ;
#5272 = EDGE_CURVE('',#4132,#4131,#3372,.T.) ;
#5273 = EDGE_CURVE('',#4112,#4132,#2505,.T.) ;
#5274 = EDGE_CURVE('',#4124,#4133,#2506,.T.) ;
#5275 = EDGE_CURVE('',#4134,#4123,#2507,.T.) ;
#5276 = EDGE_CURVE('',#4133,#4134,#3373,.T.) ;
#5277 = EDGE_CURVE('',#4135,#4107,#2508,.T.) ;
#5278 = EDGE_CURVE('',#4136,#4135,#3374,.T.) ;
#5279 = EDGE_CURVE('',#4109,#4136,#2509,.T.) ;
#5280 = EDGE_CURVE('',#4134,#4133,#2510,.T.) ;
#5281 = EDGE_CURVE('',#4122,#4137,#2511,.T.) ;
#5282 = EDGE_CURVE('',#4137,#4138,#2512,.T.) ;
#5283 = EDGE_CURVE('',#4108,#4138,#2513,.T.) ;
#5284 = EDGE_CURVE('',#4130,#4129,#2514,.T.) ;
#5285 = EDGE_CURVE('',#4119,#4139,#2515,.T.) ;
#5286 = EDGE_CURVE('',#4139,#4137,#2516,.T.) ;
#5287 = EDGE_CURVE('',#4126,#4125,#2517,.T.) ;
#5288 = EDGE_CURVE('',#4116,#4140,#2518,.T.) ;
#5289 = EDGE_CURVE('',#4140,#4139,#2519,.T.) ;
#5290 = EDGE_CURVE('',#4127,#4128,#2520,.T.) ;
#5291 = EDGE_CURVE('',#4131,#4132,#2521,.T.) ;
#5292 = EDGE_CURVE('',#4135,#4136,#2522,.T.) ;
#5293 = EDGE_CURVE('',#4141,#4142,#2523,.T.) ;
#5294 = EDGE_CURVE('',#4142,#4141,#3375,.T.) ;
#5295 = EDGE_CURVE('',#4142,#4140,#2524,.T.) ;
#5296 = EDGE_CURVE('',#4140,#4142,#3376,.T.) ;
#5297 = EDGE_CURVE('',#4139,#4140,#3377,.T.) ;
#5298 = EDGE_CURVE('',#4137,#4139,#3378,.T.) ;
#5299 = EDGE_CURVE('',#4138,#4137,#3379,.T.) ;
#5300 = EDGE_CURVE('',#4138,#4141,#2525,.T.) ;
#5301 = EDGE_CURVE('',#4141,#4138,#3380,.T.) ;
#5302 = EDGE_CURVE('',#4143,#4137,#2526,.T.) ;
#5303 = EDGE_CURVE('',#4110,#4141,#2527,.T.) ;
#5304 = EDGE_CURVE('',#4113,#4142,#2528,.T.) ;
#5305 = EDGE_CURVE('',#4144,#4144,#3381,.T.) ;
#5306 = EDGE_CURVE('',#4145,#4145,#3382,.T.) ;
#5307 = EDGE_CURVE('',#4146,#4146,#3383,.T.) ;
#5308 = EDGE_CURVE('',#4146,#4144,#2529,.T.) ;
#5309 = EDGE_CURVE('',#4147,#4147,#3384,.T.) ;
#5310 = EDGE_CURVE('',#4147,#4148,#2530,.T.) ;
#5311 = EDGE_CURVE('',#4148,#4148,#3385,.T.) ;
#5312 = EDGE_CURVE('',#4148,#4149,#2531,.T.) ;
#5313 = EDGE_CURVE('',#4149,#4149,#3386,.T.) ;
#5314 = EDGE_CURVE('',#4149,#4150,#2532,.T.) ;
#5315 = EDGE_CURVE('',#4150,#4150,#3387,.T.) ;
#5316 = EDGE_CURVE('',#4150,#4151,#2533,.T.) ;
#5317 = EDGE_CURVE('',#4151,#4151,#3388,.T.) ;
#5318 = EDGE_CURVE('',#4151,#4152,#2534,.T.) ;
#5319 = EDGE_CURVE('',#4152,#4152,#3389,.T.) ;
#5320 = EDGE_CURVE('',#4152,#4145,#2535,.T.) ;
#5321 = EDGE_CURVE('',#4153,#4153,#3390,.T.) ;
#5322 = EDGE_CURVE('',#4153,#4154,#2536,.T.) ;
#5323 = EDGE_CURVE('',#4154,#4154,#3391,.T.) ;
#5324 = EDGE_CURVE('',#4155,#4156,#2537,.T.) ;
#5325 = EDGE_CURVE('',#4157,#4155,#2538,.T.) ;
#5326 = EDGE_CURVE('',#4158,#4157,#2539,.T.) ;
#5327 = EDGE_CURVE('',#4156,#4158,#2540,.T.) ;
#5328 = EDGE_CURVE('',#4158,#4159,#2541,.T.) ;
#5329 = EDGE_CURVE('',#4160,#4157,#2542,.T.) ;
#5330 = EDGE_CURVE('',#4159,#4160,#2543,.T.) ;
#5331 = EDGE_CURVE('',#4161,#4160,#2544,.T.) ;
#5332 = EDGE_CURVE('',#4162,#4161,#2545,.T.) ;
#5333 = EDGE_CURVE('',#4159,#4162,#2546,.T.) ;
#5334 = EDGE_CURVE('',#4155,#4163,#3392,.T.) ;
#5335 = EDGE_CURVE('',#4163,#4164,#2547,.T.) ;
#5336 = EDGE_CURVE('',#4164,#4165,#2548,.T.) ;
#5337 = EDGE_CURVE('',#4165,#4166,#2549,.T.) ;
#5338 = EDGE_CURVE('',#4166,#4161,#3393,.T.) ;
#5339 = EDGE_CURVE('',#4167,#4167,#3394,.T.) ;
#5340 = EDGE_CURVE('',#4168,#4168,#3395,.T.) ;
#5341 = EDGE_CURVE('',#4168,#4167,#2550,.T.) ;
#5342 = EDGE_CURVE('',#4169,#4163,#2551,.T.) ;
#5343 = EDGE_CURVE('',#4169,#4170,#2552,.T.) ;
#5344 = EDGE_CURVE('',#4170,#4164,#2553,.T.) ;
#5345 = EDGE_CURVE('',#4170,#4171,#2554,.T.) ;
#5346 = EDGE_CURVE('',#4171,#4165,#2555,.T.) ;
#5347 = EDGE_CURVE('',#4156,#4169,#3396,.T.) ;
#5348 = EDGE_CURVE('',#4172,#4171,#2556,.T.) ;
#5349 = EDGE_CURVE('',#4166,#4172,#2557,.T.) ;
#5350 = EDGE_CURVE('',#4172,#4162,#3397,.T.) ;
#5351 = ORIENTED_EDGE('',*,*,#4173,.T.) ;
#5352 = ORIENTED_EDGE('',*,*,#4174,.T.) ;
#5353 = ORIENTED_EDGE('',*,*,#4175,.T.) ;
#5354 = ORIENTED_EDGE('',*,*,#4174,.F.) ;
#5355 = ORIENTED_EDGE('',*,*,#4175,.F.) ;
#5356 = ORIENTED_EDGE('',*,*,#4176,.T.) ;
#5357 = ORIENTED_EDGE('',*,*,#4177,.T.) ;
#5358 = ORIENTED_EDGE('',*,*,#4178,.T.) ;
#5359 = ORIENTED_EDGE('',*,*,#4176,.F.) ;
#5360 = ORIENTED_EDGE('',*,*,#4179,.T.) ;
#5361 = ORIENTED_EDGE('',*,*,#4173,.F.) ;
#5362 = ORIENTED_EDGE('',*,*,#4180,.T.) ;
#5363 = ORIENTED_EDGE('',*,*,#4177,.F.) ;
#5364 = ORIENTED_EDGE('',*,*,#4178,.F.) ;
#5365 = ORIENTED_EDGE('',*,*,#4180,.F.) ;
#5366 = ORIENTED_EDGE('',*,*,#4181,.T.) ;
#5367 = ORIENTED_EDGE('',*,*,#4182,.T.) ;
#5368 = ORIENTED_EDGE('',*,*,#4183,.T.) ;
#5369 = ORIENTED_EDGE('',*,*,#4182,.F.) ;
#5370 = ORIENTED_EDGE('',*,*,#4183,.F.) ;
#5371 = ORIENTED_EDGE('',*,*,#4184,.T.) ;
#5372 = ORIENTED_EDGE('',*,*,#4185,.T.) ;
#5373 = ORIENTED_EDGE('',*,*,#4186,.T.) ;
#5374 = ORIENTED_EDGE('',*,*,#4184,.F.) ;
#5375 = ORIENTED_EDGE('',*,*,#4187,.F.) ;
#5376 = ORIENTED_EDGE('',*,*,#4181,.F.) ;
#5377 = ORIENTED_EDGE('',*,*,#4186,.F.) ;
#5378 = ORIENTED_EDGE('',*,*,#4188,.T.) ;
#5379 = ORIENTED_EDGE('',*,*,#4188,.F.) ;
#5380 = ORIENTED_EDGE('',*,*,#4185,.F.) ;
#5381 = ORIENTED_EDGE('',*,*,#4189,.F.) ;
#5382 = ORIENTED_EDGE('',*,*,#4190,.F.) ;
#5383 = ORIENTED_EDGE('',*,*,#4191,.F.) ;
#5384 = ORIENTED_EDGE('',*,*,#4192,.F.) ;
#5385 = ORIENTED_EDGE('',*,*,#4193,.T.) ;
#5386 = ORIENTED_EDGE('',*,*,#4194,.F.) ;
#5387 = ORIENTED_EDGE('',*,*,#4190,.T.) ;
#5388 = ORIENTED_EDGE('',*,*,#4195,.F.) ;
#5389 = ORIENTED_EDGE('',*,*,#4193,.F.) ;
#5390 = ORIENTED_EDGE('',*,*,#4196,.F.) ;
#5391 = ORIENTED_EDGE('',*,*,#4197,.F.) ;
#5392 = ORIENTED_EDGE('',*,*,#4198,.T.) ;
#5393 = ORIENTED_EDGE('',*,*,#4199,.F.) ;
#5394 = ORIENTED_EDGE('',*,*,#4200,.T.) ;
#5395 = ORIENTED_EDGE('',*,*,#4201,.F.) ;
#5396 = ORIENTED_EDGE('',*,*,#4198,.F.) ;
#5397 = ORIENTED_EDGE('',*,*,#4202,.F.) ;
#5398 = ORIENTED_EDGE('',*,*,#4200,.F.) ;
#5399 = ORIENTED_EDGE('',*,*,#4203,.F.) ;
#5400 = ORIENTED_EDGE('',*,*,#4204,.F.) ;
#5401 = ORIENTED_EDGE('',*,*,#4205,.F.) ;
#5402 = ORIENTED_EDGE('',*,*,#4206,.F.) ;
#5403 = ORIENTED_EDGE('',*,*,#4207,.F.) ;
#5404 = ORIENTED_EDGE('',*,*,#4208,.F.) ;
#5405 = ORIENTED_EDGE('',*,*,#4209,.F.) ;
#5406 = ORIENTED_EDGE('',*,*,#4210,.F.) ;
#5407 = ORIENTED_EDGE('',*,*,#4211,.F.) ;
#5408 = ORIENTED_EDGE('',*,*,#4212,.F.) ;
#5409 = ORIENTED_EDGE('',*,*,#4213,.F.) ;
#5410 = ORIENTED_EDGE('',*,*,#4214,.F.) ;
#5411 = ORIENTED_EDGE('',*,*,#4215,.F.) ;
#5412 = ORIENTED_EDGE('',*,*,#4216,.F.) ;
#5413 = ORIENTED_EDGE('',*,*,#4217,.F.) ;
#5414 = ORIENTED_EDGE('',*,*,#4218,.F.) ;
#5415 = ORIENTED_EDGE('',*,*,#4219,.F.) ;
#5416 = ORIENTED_EDGE('',*,*,#4220,.F.) ;
#5417 = ORIENTED_EDGE('',*,*,#4221,.F.) ;
#5418 = ORIENTED_EDGE('',*,*,#4222,.F.) ;
#5419 = ORIENTED_EDGE('',*,*,#4223,.F.) ;
#5420 = ORIENTED_EDGE('',*,*,#4224,.F.) ;
#5421 = ORIENTED_EDGE('',*,*,#4225,.F.) ;
#5422 = ORIENTED_EDGE('',*,*,#4226,.F.) ;
#5423 = ORIENTED_EDGE('',*,*,#4227,.F.) ;
#5424 = ORIENTED_EDGE('',*,*,#4228,.F.) ;
#5425 = ORIENTED_EDGE('',*,*,#4229,.F.) ;
#5426 = ORIENTED_EDGE('',*,*,#4230,.F.) ;
#5427 = ORIENTED_EDGE('',*,*,#4231,.F.) ;
#5428 = ORIENTED_EDGE('',*,*,#4232,.F.) ;
#5429 = ORIENTED_EDGE('',*,*,#4233,.F.) ;
#5430 = ORIENTED_EDGE('',*,*,#4234,.F.) ;
#5431 = ORIENTED_EDGE('',*,*,#4225,.T.) ;
#5432 = ORIENTED_EDGE('',*,*,#4235,.T.) ;
#5433 = ORIENTED_EDGE('',*,*,#4227,.T.) ;
#5434 = ORIENTED_EDGE('',*,*,#4236,.F.) ;
#5435 = ORIENTED_EDGE('',*,*,#4211,.T.) ;
#5436 = ORIENTED_EDGE('',*,*,#4237,.T.) ;
#5437 = ORIENTED_EDGE('',*,*,#4219,.T.) ;
#5438 = ORIENTED_EDGE('',*,*,#4238,.F.) ;
#5439 = ORIENTED_EDGE('',*,*,#4205,.T.) ;
#5440 = ORIENTED_EDGE('',*,*,#4239,.F.) ;
#5441 = ORIENTED_EDGE('',*,*,#4233,.T.) ;
#5442 = ORIENTED_EDGE('',*,*,#4240,.T.) ;
#5443 = ORIENTED_EDGE('',*,*,#4203,.T.) ;
#5444 = ORIENTED_EDGE('',*,*,#4241,.T.) ;
#5445 = ORIENTED_EDGE('',*,*,#4213,.T.) ;
#5446 = ORIENTED_EDGE('',*,*,#4242,.F.) ;
#5447 = ORIENTED_EDGE('',*,*,#4224,.T.) ;
#5448 = ORIENTED_EDGE('',*,*,#4243,.T.) ;
#5449 = ORIENTED_EDGE('',*,*,#4228,.T.) ;
#5450 = ORIENTED_EDGE('',*,*,#4235,.F.) ;
#5451 = ORIENTED_EDGE('',*,*,#4218,.T.) ;
#5452 = ORIENTED_EDGE('',*,*,#4244,.T.) ;
#5453 = ORIENTED_EDGE('',*,*,#4220,.T.) ;
#5454 = ORIENTED_EDGE('',*,*,#4237,.F.) ;
#5455 = ORIENTED_EDGE('',*,*,#4206,.T.) ;
#5456 = ORIENTED_EDGE('',*,*,#4240,.F.) ;
#5457 = ORIENTED_EDGE('',*,*,#4232,.T.) ;
#5458 = ORIENTED_EDGE('',*,*,#4245,.T.) ;
#5459 = ORIENTED_EDGE('',*,*,#4210,.T.) ;
#5460 = ORIENTED_EDGE('',*,*,#4246,.T.) ;
#5461 = ORIENTED_EDGE('',*,*,#4214,.T.) ;
#5462 = ORIENTED_EDGE('',*,*,#4241,.F.) ;
#5463 = ORIENTED_EDGE('',*,*,#4223,.T.) ;
#5464 = ORIENTED_EDGE('',*,*,#4247,.T.) ;
#5465 = ORIENTED_EDGE('',*,*,#4229,.T.) ;
#5466 = ORIENTED_EDGE('',*,*,#4243,.F.) ;
#5467 = ORIENTED_EDGE('',*,*,#4217,.T.) ;
#5468 = ORIENTED_EDGE('',*,*,#4248,.T.) ;
#5469 = ORIENTED_EDGE('',*,*,#4221,.T.) ;
#5470 = ORIENTED_EDGE('',*,*,#4244,.F.) ;
#5471 = ORIENTED_EDGE('',*,*,#4207,.T.) ;
#5472 = ORIENTED_EDGE('',*,*,#4245,.F.) ;
#5473 = ORIENTED_EDGE('',*,*,#4231,.T.) ;
#5474 = ORIENTED_EDGE('',*,*,#4249,.T.) ;
#5475 = ORIENTED_EDGE('',*,*,#4209,.T.) ;
#5476 = ORIENTED_EDGE('',*,*,#4250,.T.) ;
#5477 = ORIENTED_EDGE('',*,*,#4215,.T.) ;
#5478 = ORIENTED_EDGE('',*,*,#4246,.F.) ;
#5479 = ORIENTED_EDGE('',*,*,#4208,.T.) ;
#5480 = ORIENTED_EDGE('',*,*,#4249,.F.) ;
#5481 = ORIENTED_EDGE('',*,*,#4230,.T.) ;
#5482 = ORIENTED_EDGE('',*,*,#4247,.F.) ;
#5483 = ORIENTED_EDGE('',*,*,#4222,.T.) ;
#5484 = ORIENTED_EDGE('',*,*,#4248,.F.) ;
#5485 = ORIENTED_EDGE('',*,*,#4216,.T.) ;
#5486 = ORIENTED_EDGE('',*,*,#4250,.F.) ;
#5487 = ORIENTED_EDGE('',*,*,#4251,.T.) ;
#5488 = ORIENTED_EDGE('',*,*,#4252,.F.) ;
#5489 = ORIENTED_EDGE('',*,*,#4253,.T.) ;
#5490 = ORIENTED_EDGE('',*,*,#4187,.T.) ;
#5491 = ORIENTED_EDGE('',*,*,#4253,.F.) ;
#5492 = ORIENTED_EDGE('',*,*,#4251,.F.) ;
#5493 = ORIENTED_EDGE('',*,*,#4254,.T.) ;
#5494 = ORIENTED_EDGE('',*,*,#4252,.T.) ;
#5495 = ORIENTED_EDGE('',*,*,#4254,.F.) ;
#5496 = ORIENTED_EDGE('',*,*,#4204,.T.) ;
#5497 = ORIENTED_EDGE('',*,*,#4242,.T.) ;
#5498 = ORIENTED_EDGE('',*,*,#4212,.T.) ;
#5499 = ORIENTED_EDGE('',*,*,#4238,.T.) ;
#5500 = ORIENTED_EDGE('',*,*,#4226,.T.) ;
#5501 = ORIENTED_EDGE('',*,*,#4236,.T.) ;
#5502 = ORIENTED_EDGE('',*,*,#4234,.T.) ;
#5503 = ORIENTED_EDGE('',*,*,#4239,.T.) ;
#5504 = ORIENTED_EDGE('',*,*,#4255,.F.) ;
#5505 = ORIENTED_EDGE('',*,*,#4256,.F.) ;
#5506 = ORIENTED_EDGE('',*,*,#4257,.T.) ;
#5507 = ORIENTED_EDGE('',*,*,#4191,.T.) ;
#5508 = ORIENTED_EDGE('',*,*,#4194,.T.) ;
#5509 = ORIENTED_EDGE('',*,*,#4195,.T.) ;
#5510 = ORIENTED_EDGE('',*,*,#4258,.T.) ;
#5511 = ORIENTED_EDGE('',*,*,#4255,.T.) ;
#5512 = ORIENTED_EDGE('',*,*,#4258,.F.) ;
#5513 = ORIENTED_EDGE('',*,*,#4196,.T.) ;
#5514 = ORIENTED_EDGE('',*,*,#4192,.T.) ;
#5515 = ORIENTED_EDGE('',*,*,#4189,.T.) ;
#5516 = ORIENTED_EDGE('',*,*,#4257,.F.) ;
#5517 = ORIENTED_EDGE('',*,*,#4201,.T.) ;
#5518 = ORIENTED_EDGE('',*,*,#4202,.T.) ;
#5519 = ORIENTED_EDGE('',*,*,#4199,.T.) ;
#5520 = ORIENTED_EDGE('',*,*,#4197,.T.) ;
#5521 = ORIENTED_EDGE('',*,*,#4179,.F.) ;
#5522 = ORIENTED_EDGE('',*,*,#4259,.T.) ;
#5523 = ORIENTED_EDGE('',*,*,#4256,.T.) ;
#5524 = ORIENTED_EDGE('',*,*,#4259,.F.) ;
#5525 = ORIENTED_EDGE('',*,*,#4260,.F.) ;
#5526 = ORIENTED_EDGE('',*,*,#4261,.T.) ;
#5527 = ORIENTED_EDGE('',*,*,#4262,.T.) ;
#5528 = ORIENTED_EDGE('',*,*,#4263,.F.) ;
#5529 = ORIENTED_EDGE('',*,*,#4264,.F.) ;
#5530 = ORIENTED_EDGE('',*,*,#4263,.T.) ;
#5531 = ORIENTED_EDGE('',*,*,#4265,.T.) ;
#5532 = ORIENTED_EDGE('',*,*,#4266,.F.) ;
#5533 = ORIENTED_EDGE('',*,*,#4267,.F.) ;
#5534 = ORIENTED_EDGE('',*,*,#4266,.T.) ;
#5535 = ORIENTED_EDGE('',*,*,#4268,.T.) ;
#5536 = ORIENTED_EDGE('',*,*,#4269,.F.) ;
#5537 = ORIENTED_EDGE('',*,*,#4270,.F.) ;
#5538 = ORIENTED_EDGE('',*,*,#4269,.T.) ;
#5539 = ORIENTED_EDGE('',*,*,#4271,.T.) ;
#5540 = ORIENTED_EDGE('',*,*,#4272,.F.) ;
#5541 = ORIENTED_EDGE('',*,*,#4273,.F.) ;
#5542 = ORIENTED_EDGE('',*,*,#4274,.T.) ;
#5543 = ORIENTED_EDGE('',*,*,#4275,.T.) ;
#5544 = ORIENTED_EDGE('',*,*,#4276,.F.) ;
#5545 = ORIENTED_EDGE('',*,*,#4277,.F.) ;
#5546 = ORIENTED_EDGE('',*,*,#4276,.T.) ;
#5547 = ORIENTED_EDGE('',*,*,#4278,.T.) ;
#5548 = ORIENTED_EDGE('',*,*,#4279,.F.) ;
#5549 = ORIENTED_EDGE('',*,*,#4280,.F.) ;
#5550 = ORIENTED_EDGE('',*,*,#4279,.T.) ;
#5551 = ORIENTED_EDGE('',*,*,#4281,.T.) ;
#5552 = ORIENTED_EDGE('',*,*,#4282,.F.) ;
#5553 = ORIENTED_EDGE('',*,*,#4283,.F.) ;
#5554 = ORIENTED_EDGE('',*,*,#4282,.T.) ;
#5555 = ORIENTED_EDGE('',*,*,#4284,.T.) ;
#5556 = ORIENTED_EDGE('',*,*,#4285,.F.) ;
#5557 = ORIENTED_EDGE('',*,*,#4286,.F.) ;
#5558 = ORIENTED_EDGE('',*,*,#4285,.T.) ;
#5559 = ORIENTED_EDGE('',*,*,#4287,.T.) ;
#5560 = ORIENTED_EDGE('',*,*,#4288,.F.) ;
#5561 = ORIENTED_EDGE('',*,*,#4289,.F.) ;
#5562 = ORIENTED_EDGE('',*,*,#4288,.T.) ;
#5563 = ORIENTED_EDGE('',*,*,#4290,.T.) ;
#5564 = ORIENTED_EDGE('',*,*,#4291,.F.) ;
#5565 = ORIENTED_EDGE('',*,*,#4292,.F.) ;
#5566 = ORIENTED_EDGE('',*,*,#4291,.T.) ;
#5567 = ORIENTED_EDGE('',*,*,#4293,.T.) ;
#5568 = ORIENTED_EDGE('',*,*,#4294,.F.) ;
#5569 = ORIENTED_EDGE('',*,*,#4295,.F.) ;
#5570 = ORIENTED_EDGE('',*,*,#4294,.T.) ;
#5571 = ORIENTED_EDGE('',*,*,#4296,.T.) ;
#5572 = ORIENTED_EDGE('',*,*,#4297,.F.) ;
#5573 = ORIENTED_EDGE('',*,*,#4298,.F.) ;
#5574 = ORIENTED_EDGE('',*,*,#4297,.T.) ;
#5575 = ORIENTED_EDGE('',*,*,#4299,.T.) ;
#5576 = ORIENTED_EDGE('',*,*,#4300,.F.) ;
#5577 = ORIENTED_EDGE('',*,*,#4301,.F.) ;
#5578 = ORIENTED_EDGE('',*,*,#4272,.T.) ;
#5579 = ORIENTED_EDGE('',*,*,#4302,.T.) ;
#5580 = ORIENTED_EDGE('',*,*,#4303,.F.) ;
#5581 = ORIENTED_EDGE('',*,*,#4304,.F.) ;
#5582 = ORIENTED_EDGE('',*,*,#4305,.T.) ;
#5583 = ORIENTED_EDGE('',*,*,#4306,.T.) ;
#5584 = ORIENTED_EDGE('',*,*,#4261,.F.) ;
#5585 = ORIENTED_EDGE('',*,*,#4307,.F.) ;
#5586 = ORIENTED_EDGE('',*,*,#4308,.T.) ;
#5587 = ORIENTED_EDGE('',*,*,#4309,.T.) ;
#5588 = ORIENTED_EDGE('',*,*,#4305,.F.) ;
#5589 = ORIENTED_EDGE('',*,*,#4310,.F.) ;
#5590 = ORIENTED_EDGE('',*,*,#4311,.T.) ;
#5591 = ORIENTED_EDGE('',*,*,#4312,.T.) ;
#5592 = ORIENTED_EDGE('',*,*,#4308,.F.) ;
#5593 = ORIENTED_EDGE('',*,*,#4313,.F.) ;
#5594 = ORIENTED_EDGE('',*,*,#4303,.T.) ;
#5595 = ORIENTED_EDGE('',*,*,#4314,.T.) ;
#5596 = ORIENTED_EDGE('',*,*,#4311,.F.) ;
#5597 = ORIENTED_EDGE('',*,*,#4315,.F.) ;
#5598 = ORIENTED_EDGE('',*,*,#4300,.T.) ;
#5599 = ORIENTED_EDGE('',*,*,#4316,.T.) ;
#5600 = ORIENTED_EDGE('',*,*,#4317,.F.) ;
#5601 = ORIENTED_EDGE('',*,*,#4318,.F.) ;
#5602 = ORIENTED_EDGE('',*,*,#4319,.T.) ;
#5603 = ORIENTED_EDGE('',*,*,#4320,.T.) ;
#5604 = ORIENTED_EDGE('',*,*,#4274,.F.) ;
#5605 = ORIENTED_EDGE('',*,*,#4321,.F.) ;
#5606 = ORIENTED_EDGE('',*,*,#4322,.T.) ;
#5607 = ORIENTED_EDGE('',*,*,#4323,.T.) ;
#5608 = ORIENTED_EDGE('',*,*,#4319,.F.) ;
#5609 = ORIENTED_EDGE('',*,*,#4324,.F.) ;
#5610 = ORIENTED_EDGE('',*,*,#4325,.T.) ;
#5611 = ORIENTED_EDGE('',*,*,#4326,.T.) ;
#5612 = ORIENTED_EDGE('',*,*,#4322,.F.) ;
#5613 = ORIENTED_EDGE('',*,*,#4327,.F.) ;
#5614 = ORIENTED_EDGE('',*,*,#4328,.T.) ;
#5615 = ORIENTED_EDGE('',*,*,#4329,.T.) ;
#5616 = ORIENTED_EDGE('',*,*,#4325,.F.) ;
#5617 = ORIENTED_EDGE('',*,*,#4330,.F.) ;
#5618 = ORIENTED_EDGE('',*,*,#4331,.T.) ;
#5619 = ORIENTED_EDGE('',*,*,#4332,.T.) ;
#5620 = ORIENTED_EDGE('',*,*,#4328,.F.) ;
#5621 = ORIENTED_EDGE('',*,*,#4333,.F.) ;
#5622 = ORIENTED_EDGE('',*,*,#4334,.T.) ;
#5623 = ORIENTED_EDGE('',*,*,#4335,.T.) ;
#5624 = ORIENTED_EDGE('',*,*,#4331,.F.) ;
#5625 = ORIENTED_EDGE('',*,*,#4336,.F.) ;
#5626 = ORIENTED_EDGE('',*,*,#4337,.T.) ;
#5627 = ORIENTED_EDGE('',*,*,#4338,.T.) ;
#5628 = ORIENTED_EDGE('',*,*,#4334,.F.) ;
#5629 = ORIENTED_EDGE('',*,*,#4339,.F.) ;
#5630 = ORIENTED_EDGE('',*,*,#4340,.T.) ;
#5631 = ORIENTED_EDGE('',*,*,#4341,.T.) ;
#5632 = ORIENTED_EDGE('',*,*,#4337,.F.) ;
#5633 = ORIENTED_EDGE('',*,*,#4342,.F.) ;
#5634 = ORIENTED_EDGE('',*,*,#4317,.T.) ;
#5635 = ORIENTED_EDGE('',*,*,#4343,.T.) ;
#5636 = ORIENTED_EDGE('',*,*,#4340,.F.) ;
#5637 = ORIENTED_EDGE('',*,*,#4343,.F.) ;
#5638 = ORIENTED_EDGE('',*,*,#4316,.F.) ;
#5639 = ORIENTED_EDGE('',*,*,#4299,.F.) ;
#5640 = ORIENTED_EDGE('',*,*,#4296,.F.) ;
#5641 = ORIENTED_EDGE('',*,*,#4293,.F.) ;
#5642 = ORIENTED_EDGE('',*,*,#4290,.F.) ;
#5643 = ORIENTED_EDGE('',*,*,#4287,.F.) ;
#5644 = ORIENTED_EDGE('',*,*,#4284,.F.) ;
#5645 = ORIENTED_EDGE('',*,*,#4281,.F.) ;
#5646 = ORIENTED_EDGE('',*,*,#4278,.F.) ;
#5647 = ORIENTED_EDGE('',*,*,#4275,.F.) ;
#5648 = ORIENTED_EDGE('',*,*,#4320,.F.) ;
#5649 = ORIENTED_EDGE('',*,*,#4323,.F.) ;
#5650 = ORIENTED_EDGE('',*,*,#4326,.F.) ;
#5651 = ORIENTED_EDGE('',*,*,#4329,.F.) ;
#5652 = ORIENTED_EDGE('',*,*,#4332,.F.) ;
#5653 = ORIENTED_EDGE('',*,*,#4335,.F.) ;
#5654 = ORIENTED_EDGE('',*,*,#4338,.F.) ;
#5655 = ORIENTED_EDGE('',*,*,#4341,.F.) ;
#5656 = ORIENTED_EDGE('',*,*,#4314,.F.) ;
#5657 = ORIENTED_EDGE('',*,*,#4302,.F.) ;
#5658 = ORIENTED_EDGE('',*,*,#4271,.F.) ;
#5659 = ORIENTED_EDGE('',*,*,#4268,.F.) ;
#5660 = ORIENTED_EDGE('',*,*,#4265,.F.) ;
#5661 = ORIENTED_EDGE('',*,*,#4262,.F.) ;
#5662 = ORIENTED_EDGE('',*,*,#4306,.F.) ;
#5663 = ORIENTED_EDGE('',*,*,#4309,.F.) ;
#5664 = ORIENTED_EDGE('',*,*,#4312,.F.) ;
#5665 = ORIENTED_EDGE('',*,*,#4344,.F.) ;
#5666 = ORIENTED_EDGE('',*,*,#4345,.T.) ;
#5667 = ORIENTED_EDGE('',*,*,#4346,.T.) ;
#5668 = ORIENTED_EDGE('',*,*,#4347,.F.) ;
#5669 = ORIENTED_EDGE('',*,*,#4348,.F.) ;
#5670 = ORIENTED_EDGE('',*,*,#4347,.T.) ;
#5671 = ORIENTED_EDGE('',*,*,#4349,.T.) ;
#5672 = ORIENTED_EDGE('',*,*,#4350,.F.) ;
#5673 = ORIENTED_EDGE('',*,*,#4351,.F.) ;
#5674 = ORIENTED_EDGE('',*,*,#4350,.T.) ;
#5675 = ORIENTED_EDGE('',*,*,#4352,.T.) ;
#5676 = ORIENTED_EDGE('',*,*,#4353,.F.) ;
#5677 = ORIENTED_EDGE('',*,*,#4354,.F.) ;
#5678 = ORIENTED_EDGE('',*,*,#4353,.T.) ;
#5679 = ORIENTED_EDGE('',*,*,#4355,.T.) ;
#5680 = ORIENTED_EDGE('',*,*,#4356,.F.) ;
#5681 = ORIENTED_EDGE('',*,*,#4357,.F.) ;
#5682 = ORIENTED_EDGE('',*,*,#4356,.T.) ;
#5683 = ORIENTED_EDGE('',*,*,#4358,.T.) ;
#5684 = ORIENTED_EDGE('',*,*,#4359,.F.) ;
#5685 = ORIENTED_EDGE('',*,*,#4360,.F.) ;
#5686 = ORIENTED_EDGE('',*,*,#4361,.T.) ;
#5687 = ORIENTED_EDGE('',*,*,#4362,.T.) ;
#5688 = ORIENTED_EDGE('',*,*,#4345,.F.) ;
#5689 = ORIENTED_EDGE('',*,*,#4363,.F.) ;
#5690 = ORIENTED_EDGE('',*,*,#4364,.T.) ;
#5691 = ORIENTED_EDGE('',*,*,#4365,.T.) ;
#5692 = ORIENTED_EDGE('',*,*,#4361,.F.) ;
#5693 = ORIENTED_EDGE('',*,*,#4366,.F.) ;
#5694 = ORIENTED_EDGE('',*,*,#4367,.T.) ;
#5695 = ORIENTED_EDGE('',*,*,#4368,.T.) ;
#5696 = ORIENTED_EDGE('',*,*,#4364,.F.) ;
#5697 = ORIENTED_EDGE('',*,*,#4369,.F.) ;
#5698 = ORIENTED_EDGE('',*,*,#4359,.T.) ;
#5699 = ORIENTED_EDGE('',*,*,#4370,.T.) ;
#5700 = ORIENTED_EDGE('',*,*,#4367,.F.) ;
#5701 = ORIENTED_EDGE('',*,*,#4370,.F.) ;
#5702 = ORIENTED_EDGE('',*,*,#4358,.F.) ;
#5703 = ORIENTED_EDGE('',*,*,#4355,.F.) ;
#5704 = ORIENTED_EDGE('',*,*,#4352,.F.) ;
#5705 = ORIENTED_EDGE('',*,*,#4349,.F.) ;
#5706 = ORIENTED_EDGE('',*,*,#4346,.F.) ;
#5707 = ORIENTED_EDGE('',*,*,#4362,.F.) ;
#5708 = ORIENTED_EDGE('',*,*,#4365,.F.) ;
#5709 = ORIENTED_EDGE('',*,*,#4368,.F.) ;
#5710 = ORIENTED_EDGE('',*,*,#4371,.F.) ;
#5711 = ORIENTED_EDGE('',*,*,#4372,.T.) ;
#5712 = ORIENTED_EDGE('',*,*,#4373,.T.) ;
#5713 = ORIENTED_EDGE('',*,*,#4372,.F.) ;
#5714 = ORIENTED_EDGE('',*,*,#4374,.T.) ;
#5715 = ORIENTED_EDGE('',*,*,#4375,.T.) ;
#5716 = ORIENTED_EDGE('',*,*,#4376,.T.) ;
#5717 = ORIENTED_EDGE('',*,*,#4377,.T.) ;
#5718 = ORIENTED_EDGE('',*,*,#4378,.T.) ;
#5719 = ORIENTED_EDGE('',*,*,#4379,.T.) ;
#5720 = ORIENTED_EDGE('',*,*,#4380,.T.) ;
#5721 = ORIENTED_EDGE('',*,*,#4381,.T.) ;
#5722 = ORIENTED_EDGE('',*,*,#4382,.T.) ;
#5723 = ORIENTED_EDGE('',*,*,#4383,.T.) ;
#5724 = ORIENTED_EDGE('',*,*,#4384,.T.) ;
#5725 = ORIENTED_EDGE('',*,*,#4385,.T.) ;
#5726 = ORIENTED_EDGE('',*,*,#4386,.T.) ;
#5727 = ORIENTED_EDGE('',*,*,#4387,.T.) ;
#5728 = ORIENTED_EDGE('',*,*,#4388,.T.) ;
#5729 = ORIENTED_EDGE('',*,*,#4389,.T.) ;
#5730 = ORIENTED_EDGE('',*,*,#4390,.T.) ;
#5731 = ORIENTED_EDGE('',*,*,#4391,.T.) ;
#5732 = ORIENTED_EDGE('',*,*,#4392,.T.) ;
#5733 = ORIENTED_EDGE('',*,*,#4393,.T.) ;
#5734 = ORIENTED_EDGE('',*,*,#4394,.T.) ;
#5735 = ORIENTED_EDGE('',*,*,#4395,.T.) ;
#5736 = ORIENTED_EDGE('',*,*,#4396,.T.) ;
#5737 = ORIENTED_EDGE('',*,*,#4397,.T.) ;
#5738 = ORIENTED_EDGE('',*,*,#4398,.T.) ;
#5739 = ORIENTED_EDGE('',*,*,#4399,.T.) ;
#5740 = ORIENTED_EDGE('',*,*,#4400,.T.) ;
#5741 = ORIENTED_EDGE('',*,*,#4401,.T.) ;
#5742 = ORIENTED_EDGE('',*,*,#4402,.T.) ;
#5743 = ORIENTED_EDGE('',*,*,#4403,.T.) ;
#5744 = ORIENTED_EDGE('',*,*,#4404,.T.) ;
#5745 = ORIENTED_EDGE('',*,*,#4405,.T.) ;
#5746 = ORIENTED_EDGE('',*,*,#4406,.T.) ;
#5747 = ORIENTED_EDGE('',*,*,#4407,.T.) ;
#5748 = ORIENTED_EDGE('',*,*,#4408,.T.) ;
#5749 = ORIENTED_EDGE('',*,*,#4409,.T.) ;
#5750 = ORIENTED_EDGE('',*,*,#4410,.T.) ;
#5751 = ORIENTED_EDGE('',*,*,#4411,.T.) ;
#5752 = ORIENTED_EDGE('',*,*,#4412,.T.) ;
#5753 = ORIENTED_EDGE('',*,*,#4413,.T.) ;
#5754 = ORIENTED_EDGE('',*,*,#4414,.T.) ;
#5755 = ORIENTED_EDGE('',*,*,#4415,.T.) ;
#5756 = ORIENTED_EDGE('',*,*,#4416,.T.) ;
#5757 = ORIENTED_EDGE('',*,*,#4417,.T.) ;
#5758 = ORIENTED_EDGE('',*,*,#4418,.T.) ;
#5759 = ORIENTED_EDGE('',*,*,#4419,.T.) ;
#5760 = ORIENTED_EDGE('',*,*,#4420,.T.) ;
#5761 = ORIENTED_EDGE('',*,*,#4421,.T.) ;
#5762 = ORIENTED_EDGE('',*,*,#4422,.T.) ;
#5763 = ORIENTED_EDGE('',*,*,#4423,.T.) ;
#5764 = ORIENTED_EDGE('',*,*,#4424,.T.) ;
#5765 = ORIENTED_EDGE('',*,*,#4425,.T.) ;
#5766 = ORIENTED_EDGE('',*,*,#4426,.T.) ;
#5767 = ORIENTED_EDGE('',*,*,#4427,.T.) ;
#5768 = ORIENTED_EDGE('',*,*,#4428,.T.) ;
#5769 = ORIENTED_EDGE('',*,*,#4429,.T.) ;
#5770 = ORIENTED_EDGE('',*,*,#4430,.T.) ;
#5771 = ORIENTED_EDGE('',*,*,#4431,.T.) ;
#5772 = ORIENTED_EDGE('',*,*,#4432,.T.) ;
#5773 = ORIENTED_EDGE('',*,*,#4433,.T.) ;
#5774 = ORIENTED_EDGE('',*,*,#4434,.T.) ;
#5775 = ORIENTED_EDGE('',*,*,#4435,.T.) ;
#5776 = ORIENTED_EDGE('',*,*,#4436,.T.) ;
#5777 = ORIENTED_EDGE('',*,*,#4437,.T.) ;
#5778 = ORIENTED_EDGE('',*,*,#4438,.T.) ;
#5779 = ORIENTED_EDGE('',*,*,#4439,.T.) ;
#5780 = ORIENTED_EDGE('',*,*,#4440,.T.) ;
#5781 = ORIENTED_EDGE('',*,*,#4441,.T.) ;
#5782 = ORIENTED_EDGE('',*,*,#4442,.T.) ;
#5783 = ORIENTED_EDGE('',*,*,#4443,.T.) ;
#5784 = ORIENTED_EDGE('',*,*,#4444,.T.) ;
#5785 = ORIENTED_EDGE('',*,*,#4445,.T.) ;
#5786 = ORIENTED_EDGE('',*,*,#4446,.T.) ;
#5787 = ORIENTED_EDGE('',*,*,#4447,.T.) ;
#5788 = ORIENTED_EDGE('',*,*,#4448,.T.) ;
#5789 = ORIENTED_EDGE('',*,*,#4449,.T.) ;
#5790 = ORIENTED_EDGE('',*,*,#4450,.T.) ;
#5791 = ORIENTED_EDGE('',*,*,#4451,.T.) ;
#5792 = ORIENTED_EDGE('',*,*,#4452,.T.) ;
#5793 = ORIENTED_EDGE('',*,*,#4453,.T.) ;
#5794 = ORIENTED_EDGE('',*,*,#4454,.T.) ;
#5795 = ORIENTED_EDGE('',*,*,#4455,.T.) ;
#5796 = ORIENTED_EDGE('',*,*,#4456,.T.) ;
#5797 = ORIENTED_EDGE('',*,*,#4457,.T.) ;
#5798 = ORIENTED_EDGE('',*,*,#4458,.T.) ;
#5799 = ORIENTED_EDGE('',*,*,#4459,.T.) ;
#5800 = ORIENTED_EDGE('',*,*,#4460,.T.) ;
#5801 = ORIENTED_EDGE('',*,*,#4461,.T.) ;
#5802 = ORIENTED_EDGE('',*,*,#4462,.T.) ;
#5803 = ORIENTED_EDGE('',*,*,#4463,.T.) ;
#5804 = ORIENTED_EDGE('',*,*,#4357,.T.) ;
#5805 = ORIENTED_EDGE('',*,*,#4369,.T.) ;
#5806 = ORIENTED_EDGE('',*,*,#4366,.T.) ;
#5807 = ORIENTED_EDGE('',*,*,#4363,.T.) ;
#5808 = ORIENTED_EDGE('',*,*,#4360,.T.) ;
#5809 = ORIENTED_EDGE('',*,*,#4344,.T.) ;
#5810 = ORIENTED_EDGE('',*,*,#4348,.T.) ;
#5811 = ORIENTED_EDGE('',*,*,#4351,.T.) ;
#5812 = ORIENTED_EDGE('',*,*,#4354,.T.) ;
#5813 = ORIENTED_EDGE('',*,*,#4315,.T.) ;
#5814 = ORIENTED_EDGE('',*,*,#4342,.T.) ;
#5815 = ORIENTED_EDGE('',*,*,#4339,.T.) ;
#5816 = ORIENTED_EDGE('',*,*,#4336,.T.) ;
#5817 = ORIENTED_EDGE('',*,*,#4333,.T.) ;
#5818 = ORIENTED_EDGE('',*,*,#4330,.T.) ;
#5819 = ORIENTED_EDGE('',*,*,#4327,.T.) ;
#5820 = ORIENTED_EDGE('',*,*,#4324,.T.) ;
#5821 = ORIENTED_EDGE('',*,*,#4321,.T.) ;
#5822 = ORIENTED_EDGE('',*,*,#4318,.T.) ;
#5823 = ORIENTED_EDGE('',*,*,#4273,.T.) ;
#5824 = ORIENTED_EDGE('',*,*,#4277,.T.) ;
#5825 = ORIENTED_EDGE('',*,*,#4280,.T.) ;
#5826 = ORIENTED_EDGE('',*,*,#4283,.T.) ;
#5827 = ORIENTED_EDGE('',*,*,#4286,.T.) ;
#5828 = ORIENTED_EDGE('',*,*,#4289,.T.) ;
#5829 = ORIENTED_EDGE('',*,*,#4292,.T.) ;
#5830 = ORIENTED_EDGE('',*,*,#4295,.T.) ;
#5831 = ORIENTED_EDGE('',*,*,#4298,.T.) ;
#5832 = ORIENTED_EDGE('',*,*,#4462,.F.) ;
#5833 = ORIENTED_EDGE('',*,*,#4464,.T.) ;
#5834 = ORIENTED_EDGE('',*,*,#4465,.T.) ;
#5835 = ORIENTED_EDGE('',*,*,#4466,.F.) ;
#5836 = ORIENTED_EDGE('',*,*,#4463,.F.) ;
#5837 = ORIENTED_EDGE('',*,*,#4466,.T.) ;
#5838 = ORIENTED_EDGE('',*,*,#4467,.T.) ;
#5839 = ORIENTED_EDGE('',*,*,#4468,.F.) ;
#5840 = ORIENTED_EDGE('',*,*,#4460,.F.) ;
#5841 = ORIENTED_EDGE('',*,*,#4468,.T.) ;
#5842 = ORIENTED_EDGE('',*,*,#4469,.T.) ;
#5843 = ORIENTED_EDGE('',*,*,#4470,.F.) ;
#5844 = ORIENTED_EDGE('',*,*,#4461,.F.) ;
#5845 = ORIENTED_EDGE('',*,*,#4470,.T.) ;
#5846 = ORIENTED_EDGE('',*,*,#4471,.T.) ;
#5847 = ORIENTED_EDGE('',*,*,#4464,.F.) ;
#5848 = ORIENTED_EDGE('',*,*,#4471,.F.) ;
#5849 = ORIENTED_EDGE('',*,*,#4469,.F.) ;
#5850 = ORIENTED_EDGE('',*,*,#4467,.F.) ;
#5851 = ORIENTED_EDGE('',*,*,#4465,.F.) ;
#5852 = ORIENTED_EDGE('',*,*,#4458,.F.) ;
#5853 = ORIENTED_EDGE('',*,*,#4472,.T.) ;
#5854 = ORIENTED_EDGE('',*,*,#4473,.T.) ;
#5855 = ORIENTED_EDGE('',*,*,#4474,.F.) ;
#5856 = ORIENTED_EDGE('',*,*,#4459,.F.) ;
#5857 = ORIENTED_EDGE('',*,*,#4474,.T.) ;
#5858 = ORIENTED_EDGE('',*,*,#4475,.T.) ;
#5859 = ORIENTED_EDGE('',*,*,#4476,.F.) ;
#5860 = ORIENTED_EDGE('',*,*,#4456,.F.) ;
#5861 = ORIENTED_EDGE('',*,*,#4476,.T.) ;
#5862 = ORIENTED_EDGE('',*,*,#4477,.T.) ;
#5863 = ORIENTED_EDGE('',*,*,#4478,.F.) ;
#5864 = ORIENTED_EDGE('',*,*,#4457,.F.) ;
#5865 = ORIENTED_EDGE('',*,*,#4478,.T.) ;
#5866 = ORIENTED_EDGE('',*,*,#4479,.T.) ;
#5867 = ORIENTED_EDGE('',*,*,#4472,.F.) ;
#5868 = ORIENTED_EDGE('',*,*,#4479,.F.) ;
#5869 = ORIENTED_EDGE('',*,*,#4477,.F.) ;
#5870 = ORIENTED_EDGE('',*,*,#4475,.F.) ;
#5871 = ORIENTED_EDGE('',*,*,#4473,.F.) ;
#5872 = ORIENTED_EDGE('',*,*,#4449,.F.) ;
#5873 = ORIENTED_EDGE('',*,*,#4480,.T.) ;
#5874 = ORIENTED_EDGE('',*,*,#4481,.T.) ;
#5875 = ORIENTED_EDGE('',*,*,#4482,.F.) ;
#5876 = ORIENTED_EDGE('',*,*,#4450,.F.) ;
#5877 = ORIENTED_EDGE('',*,*,#4482,.T.) ;
#5878 = ORIENTED_EDGE('',*,*,#4483,.T.) ;
#5879 = ORIENTED_EDGE('',*,*,#4484,.F.) ;
#5880 = ORIENTED_EDGE('',*,*,#4451,.F.) ;
#5881 = ORIENTED_EDGE('',*,*,#4484,.T.) ;
#5882 = ORIENTED_EDGE('',*,*,#4485,.T.) ;
#5883 = ORIENTED_EDGE('',*,*,#4486,.F.) ;
#5884 = ORIENTED_EDGE('',*,*,#4452,.F.) ;
#5885 = ORIENTED_EDGE('',*,*,#4486,.T.) ;
#5886 = ORIENTED_EDGE('',*,*,#4487,.T.) ;
#5887 = ORIENTED_EDGE('',*,*,#4488,.F.) ;
#5888 = ORIENTED_EDGE('',*,*,#4453,.F.) ;
#5889 = ORIENTED_EDGE('',*,*,#4488,.T.) ;
#5890 = ORIENTED_EDGE('',*,*,#4489,.T.) ;
#5891 = ORIENTED_EDGE('',*,*,#4490,.F.) ;
#5892 = ORIENTED_EDGE('',*,*,#4454,.F.) ;
#5893 = ORIENTED_EDGE('',*,*,#4490,.T.) ;
#5894 = ORIENTED_EDGE('',*,*,#4491,.T.) ;
#5895 = ORIENTED_EDGE('',*,*,#4492,.F.) ;
#5896 = ORIENTED_EDGE('',*,*,#4455,.F.) ;
#5897 = ORIENTED_EDGE('',*,*,#4492,.T.) ;
#5898 = ORIENTED_EDGE('',*,*,#4493,.T.) ;
#5899 = ORIENTED_EDGE('',*,*,#4494,.F.) ;
#5900 = ORIENTED_EDGE('',*,*,#4441,.F.) ;
#5901 = ORIENTED_EDGE('',*,*,#4494,.T.) ;
#5902 = ORIENTED_EDGE('',*,*,#4495,.T.) ;
#5903 = ORIENTED_EDGE('',*,*,#4496,.F.) ;
#5904 = ORIENTED_EDGE('',*,*,#4448,.F.) ;
#5905 = ORIENTED_EDGE('',*,*,#4497,.T.) ;
#5906 = ORIENTED_EDGE('',*,*,#4498,.T.) ;
#5907 = ORIENTED_EDGE('',*,*,#4480,.F.) ;
#5908 = ORIENTED_EDGE('',*,*,#4447,.F.) ;
#5909 = ORIENTED_EDGE('',*,*,#4499,.T.) ;
#5910 = ORIENTED_EDGE('',*,*,#4500,.T.) ;
#5911 = ORIENTED_EDGE('',*,*,#4497,.F.) ;
#5912 = ORIENTED_EDGE('',*,*,#4446,.F.) ;
#5913 = ORIENTED_EDGE('',*,*,#4501,.T.) ;
#5914 = ORIENTED_EDGE('',*,*,#4502,.T.) ;
#5915 = ORIENTED_EDGE('',*,*,#4499,.F.) ;
#5916 = ORIENTED_EDGE('',*,*,#4445,.F.) ;
#5917 = ORIENTED_EDGE('',*,*,#4503,.T.) ;
#5918 = ORIENTED_EDGE('',*,*,#4504,.T.) ;
#5919 = ORIENTED_EDGE('',*,*,#4501,.F.) ;
#5920 = ORIENTED_EDGE('',*,*,#4444,.F.) ;
#5921 = ORIENTED_EDGE('',*,*,#4505,.T.) ;
#5922 = ORIENTED_EDGE('',*,*,#4506,.T.) ;
#5923 = ORIENTED_EDGE('',*,*,#4503,.F.) ;
#5924 = ORIENTED_EDGE('',*,*,#4443,.F.) ;
#5925 = ORIENTED_EDGE('',*,*,#4507,.T.) ;
#5926 = ORIENTED_EDGE('',*,*,#4508,.T.) ;
#5927 = ORIENTED_EDGE('',*,*,#4505,.F.) ;
#5928 = ORIENTED_EDGE('',*,*,#4442,.F.) ;
#5929 = ORIENTED_EDGE('',*,*,#4496,.T.) ;
#5930 = ORIENTED_EDGE('',*,*,#4509,.T.) ;
#5931 = ORIENTED_EDGE('',*,*,#4507,.F.) ;
#5932 = ORIENTED_EDGE('',*,*,#4509,.F.) ;
#5933 = ORIENTED_EDGE('',*,*,#4495,.F.) ;
#5934 = ORIENTED_EDGE('',*,*,#4493,.F.) ;
#5935 = ORIENTED_EDGE('',*,*,#4491,.F.) ;
#5936 = ORIENTED_EDGE('',*,*,#4489,.F.) ;
#5937 = ORIENTED_EDGE('',*,*,#4487,.F.) ;
#5938 = ORIENTED_EDGE('',*,*,#4485,.F.) ;
#5939 = ORIENTED_EDGE('',*,*,#4483,.F.) ;
#5940 = ORIENTED_EDGE('',*,*,#4481,.F.) ;
#5941 = ORIENTED_EDGE('',*,*,#4498,.F.) ;
#5942 = ORIENTED_EDGE('',*,*,#4500,.F.) ;
#5943 = ORIENTED_EDGE('',*,*,#4502,.F.) ;
#5944 = ORIENTED_EDGE('',*,*,#4504,.F.) ;
#5945 = ORIENTED_EDGE('',*,*,#4506,.F.) ;
#5946 = ORIENTED_EDGE('',*,*,#4508,.F.) ;
#5947 = ORIENTED_EDGE('',*,*,#4433,.F.) ;
#5948 = ORIENTED_EDGE('',*,*,#4510,.T.) ;
#5949 = ORIENTED_EDGE('',*,*,#4511,.T.) ;
#5950 = ORIENTED_EDGE('',*,*,#4512,.F.) ;
#5951 = ORIENTED_EDGE('',*,*,#4434,.F.) ;
#5952 = ORIENTED_EDGE('',*,*,#4512,.T.) ;
#5953 = ORIENTED_EDGE('',*,*,#4513,.T.) ;
#5954 = ORIENTED_EDGE('',*,*,#4514,.F.) ;
#5955 = ORIENTED_EDGE('',*,*,#4435,.F.) ;
#5956 = ORIENTED_EDGE('',*,*,#4514,.T.) ;
#5957 = ORIENTED_EDGE('',*,*,#4515,.T.) ;
#5958 = ORIENTED_EDGE('',*,*,#4516,.F.) ;
#5959 = ORIENTED_EDGE('',*,*,#4436,.F.) ;
#5960 = ORIENTED_EDGE('',*,*,#4516,.T.) ;
#5961 = ORIENTED_EDGE('',*,*,#4517,.T.) ;
#5962 = ORIENTED_EDGE('',*,*,#4518,.F.) ;
#5963 = ORIENTED_EDGE('',*,*,#4437,.F.) ;
#5964 = ORIENTED_EDGE('',*,*,#4518,.T.) ;
#5965 = ORIENTED_EDGE('',*,*,#4519,.T.) ;
#5966 = ORIENTED_EDGE('',*,*,#4520,.F.) ;
#5967 = ORIENTED_EDGE('',*,*,#4438,.F.) ;
#5968 = ORIENTED_EDGE('',*,*,#4520,.T.) ;
#5969 = ORIENTED_EDGE('',*,*,#4521,.T.) ;
#5970 = ORIENTED_EDGE('',*,*,#4522,.F.) ;
#5971 = ORIENTED_EDGE('',*,*,#4439,.F.) ;
#5972 = ORIENTED_EDGE('',*,*,#4522,.T.) ;
#5973 = ORIENTED_EDGE('',*,*,#4523,.T.) ;
#5974 = ORIENTED_EDGE('',*,*,#4524,.F.) ;
#5975 = ORIENTED_EDGE('',*,*,#4440,.F.) ;
#5976 = ORIENTED_EDGE('',*,*,#4524,.T.) ;
#5977 = ORIENTED_EDGE('',*,*,#4525,.T.) ;
#5978 = ORIENTED_EDGE('',*,*,#4526,.F.) ;
#5979 = ORIENTED_EDGE('',*,*,#4424,.F.) ;
#5980 = ORIENTED_EDGE('',*,*,#4526,.T.) ;
#5981 = ORIENTED_EDGE('',*,*,#4527,.T.) ;
#5982 = ORIENTED_EDGE('',*,*,#4528,.F.) ;
#5983 = ORIENTED_EDGE('',*,*,#4432,.F.) ;
#5984 = ORIENTED_EDGE('',*,*,#4529,.T.) ;
#5985 = ORIENTED_EDGE('',*,*,#4530,.T.) ;
#5986 = ORIENTED_EDGE('',*,*,#4510,.F.) ;
#5987 = ORIENTED_EDGE('',*,*,#4431,.F.) ;
#5988 = ORIENTED_EDGE('',*,*,#4531,.T.) ;
#5989 = ORIENTED_EDGE('',*,*,#4532,.T.) ;
#5990 = ORIENTED_EDGE('',*,*,#4529,.F.) ;
#5991 = ORIENTED_EDGE('',*,*,#4430,.F.) ;
#5992 = ORIENTED_EDGE('',*,*,#4533,.T.) ;
#5993 = ORIENTED_EDGE('',*,*,#4534,.T.) ;
#5994 = ORIENTED_EDGE('',*,*,#4531,.F.) ;
#5995 = ORIENTED_EDGE('',*,*,#4429,.F.) ;
#5996 = ORIENTED_EDGE('',*,*,#4535,.T.) ;
#5997 = ORIENTED_EDGE('',*,*,#4536,.T.) ;
#5998 = ORIENTED_EDGE('',*,*,#4533,.F.) ;
#5999 = ORIENTED_EDGE('',*,*,#4428,.F.) ;
#6000 = ORIENTED_EDGE('',*,*,#4537,.T.) ;
#6001 = ORIENTED_EDGE('',*,*,#4538,.T.) ;
#6002 = ORIENTED_EDGE('',*,*,#4535,.F.) ;
#6003 = ORIENTED_EDGE('',*,*,#4427,.F.) ;
#6004 = ORIENTED_EDGE('',*,*,#4539,.T.) ;
#6005 = ORIENTED_EDGE('',*,*,#4540,.T.) ;
#6006 = ORIENTED_EDGE('',*,*,#4537,.F.) ;
#6007 = ORIENTED_EDGE('',*,*,#4426,.F.) ;
#6008 = ORIENTED_EDGE('',*,*,#4541,.T.) ;
#6009 = ORIENTED_EDGE('',*,*,#4542,.T.) ;
#6010 = ORIENTED_EDGE('',*,*,#4539,.F.) ;
#6011 = ORIENTED_EDGE('',*,*,#4425,.F.) ;
#6012 = ORIENTED_EDGE('',*,*,#4528,.T.) ;
#6013 = ORIENTED_EDGE('',*,*,#4543,.T.) ;
#6014 = ORIENTED_EDGE('',*,*,#4541,.F.) ;
#6015 = ORIENTED_EDGE('',*,*,#4543,.F.) ;
#6016 = ORIENTED_EDGE('',*,*,#4527,.F.) ;
#6017 = ORIENTED_EDGE('',*,*,#4525,.F.) ;
#6018 = ORIENTED_EDGE('',*,*,#4523,.F.) ;
#6019 = ORIENTED_EDGE('',*,*,#4521,.F.) ;
#6020 = ORIENTED_EDGE('',*,*,#4519,.F.) ;
#6021 = ORIENTED_EDGE('',*,*,#4517,.F.) ;
#6022 = ORIENTED_EDGE('',*,*,#4515,.F.) ;
#6023 = ORIENTED_EDGE('',*,*,#4513,.F.) ;
#6024 = ORIENTED_EDGE('',*,*,#4511,.F.) ;
#6025 = ORIENTED_EDGE('',*,*,#4530,.F.) ;
#6026 = ORIENTED_EDGE('',*,*,#4532,.F.) ;
#6027 = ORIENTED_EDGE('',*,*,#4534,.F.) ;
#6028 = ORIENTED_EDGE('',*,*,#4536,.F.) ;
#6029 = ORIENTED_EDGE('',*,*,#4538,.F.) ;
#6030 = ORIENTED_EDGE('',*,*,#4540,.F.) ;
#6031 = ORIENTED_EDGE('',*,*,#4542,.F.) ;
#6032 = ORIENTED_EDGE('',*,*,#4407,.F.) ;
#6033 = ORIENTED_EDGE('',*,*,#4544,.T.) ;
#6034 = ORIENTED_EDGE('',*,*,#4545,.T.) ;
#6035 = ORIENTED_EDGE('',*,*,#4546,.F.) ;
#6036 = ORIENTED_EDGE('',*,*,#4408,.F.) ;
#6037 = ORIENTED_EDGE('',*,*,#4546,.T.) ;
#6038 = ORIENTED_EDGE('',*,*,#4547,.T.) ;
#6039 = ORIENTED_EDGE('',*,*,#4548,.F.) ;
#6040 = ORIENTED_EDGE('',*,*,#4409,.F.) ;
#6041 = ORIENTED_EDGE('',*,*,#4548,.T.) ;
#6042 = ORIENTED_EDGE('',*,*,#4549,.T.) ;
#6043 = ORIENTED_EDGE('',*,*,#4550,.F.) ;
#6044 = ORIENTED_EDGE('',*,*,#4410,.F.) ;
#6045 = ORIENTED_EDGE('',*,*,#4550,.T.) ;
#6046 = ORIENTED_EDGE('',*,*,#4551,.T.) ;
#6047 = ORIENTED_EDGE('',*,*,#4552,.F.) ;
#6048 = ORIENTED_EDGE('',*,*,#4411,.F.) ;
#6049 = ORIENTED_EDGE('',*,*,#4552,.T.) ;
#6050 = ORIENTED_EDGE('',*,*,#4553,.T.) ;
#6051 = ORIENTED_EDGE('',*,*,#4554,.F.) ;
#6052 = ORIENTED_EDGE('',*,*,#4412,.F.) ;
#6053 = ORIENTED_EDGE('',*,*,#4554,.T.) ;
#6054 = ORIENTED_EDGE('',*,*,#4555,.T.) ;
#6055 = ORIENTED_EDGE('',*,*,#4556,.F.) ;
#6056 = ORIENTED_EDGE('',*,*,#4413,.F.) ;
#6057 = ORIENTED_EDGE('',*,*,#4556,.T.) ;
#6058 = ORIENTED_EDGE('',*,*,#4557,.T.) ;
#6059 = ORIENTED_EDGE('',*,*,#4558,.F.) ;
#6060 = ORIENTED_EDGE('',*,*,#4414,.F.) ;
#6061 = ORIENTED_EDGE('',*,*,#4558,.T.) ;
#6062 = ORIENTED_EDGE('',*,*,#4559,.T.) ;
#6063 = ORIENTED_EDGE('',*,*,#4560,.F.) ;
#6064 = ORIENTED_EDGE('',*,*,#4415,.F.) ;
#6065 = ORIENTED_EDGE('',*,*,#4560,.T.) ;
#6066 = ORIENTED_EDGE('',*,*,#4561,.T.) ;
#6067 = ORIENTED_EDGE('',*,*,#4562,.F.) ;
#6068 = ORIENTED_EDGE('',*,*,#4416,.F.) ;
#6069 = ORIENTED_EDGE('',*,*,#4562,.T.) ;
#6070 = ORIENTED_EDGE('',*,*,#4563,.T.) ;
#6071 = ORIENTED_EDGE('',*,*,#4564,.F.) ;
#6072 = ORIENTED_EDGE('',*,*,#4417,.F.) ;
#6073 = ORIENTED_EDGE('',*,*,#4564,.T.) ;
#6074 = ORIENTED_EDGE('',*,*,#4565,.T.) ;
#6075 = ORIENTED_EDGE('',*,*,#4566,.F.) ;
#6076 = ORIENTED_EDGE('',*,*,#4418,.F.) ;
#6077 = ORIENTED_EDGE('',*,*,#4566,.T.) ;
#6078 = ORIENTED_EDGE('',*,*,#4567,.T.) ;
#6079 = ORIENTED_EDGE('',*,*,#4568,.F.) ;
#6080 = ORIENTED_EDGE('',*,*,#4419,.F.) ;
#6081 = ORIENTED_EDGE('',*,*,#4568,.T.) ;
#6082 = ORIENTED_EDGE('',*,*,#4569,.T.) ;
#6083 = ORIENTED_EDGE('',*,*,#4570,.F.) ;
#6084 = ORIENTED_EDGE('',*,*,#4420,.F.) ;
#6085 = ORIENTED_EDGE('',*,*,#4570,.T.) ;
#6086 = ORIENTED_EDGE('',*,*,#4571,.T.) ;
#6087 = ORIENTED_EDGE('',*,*,#4572,.F.) ;
#6088 = ORIENTED_EDGE('',*,*,#4421,.F.) ;
#6089 = ORIENTED_EDGE('',*,*,#4572,.T.) ;
#6090 = ORIENTED_EDGE('',*,*,#4573,.T.) ;
#6091 = ORIENTED_EDGE('',*,*,#4574,.F.) ;
#6092 = ORIENTED_EDGE('',*,*,#4422,.F.) ;
#6093 = ORIENTED_EDGE('',*,*,#4574,.T.) ;
#6094 = ORIENTED_EDGE('',*,*,#4575,.T.) ;
#6095 = ORIENTED_EDGE('',*,*,#4576,.F.) ;
#6096 = ORIENTED_EDGE('',*,*,#4423,.F.) ;
#6097 = ORIENTED_EDGE('',*,*,#4576,.T.) ;
#6098 = ORIENTED_EDGE('',*,*,#4577,.T.) ;
#6099 = ORIENTED_EDGE('',*,*,#4578,.F.) ;
#6100 = ORIENTED_EDGE('',*,*,#4389,.F.) ;
#6101 = ORIENTED_EDGE('',*,*,#4578,.T.) ;
#6102 = ORIENTED_EDGE('',*,*,#4579,.T.) ;
#6103 = ORIENTED_EDGE('',*,*,#4580,.F.) ;
#6104 = ORIENTED_EDGE('',*,*,#4406,.F.) ;
#6105 = ORIENTED_EDGE('',*,*,#4581,.T.) ;
#6106 = ORIENTED_EDGE('',*,*,#4582,.T.) ;
#6107 = ORIENTED_EDGE('',*,*,#4544,.F.) ;
#6108 = ORIENTED_EDGE('',*,*,#4405,.F.) ;
#6109 = ORIENTED_EDGE('',*,*,#4583,.T.) ;
#6110 = ORIENTED_EDGE('',*,*,#4584,.T.) ;
#6111 = ORIENTED_EDGE('',*,*,#4581,.F.) ;
#6112 = ORIENTED_EDGE('',*,*,#4404,.F.) ;
#6113 = ORIENTED_EDGE('',*,*,#4585,.T.) ;
#6114 = ORIENTED_EDGE('',*,*,#4586,.T.) ;
#6115 = ORIENTED_EDGE('',*,*,#4583,.F.) ;
#6116 = ORIENTED_EDGE('',*,*,#4403,.F.) ;
#6117 = ORIENTED_EDGE('',*,*,#4587,.T.) ;
#6118 = ORIENTED_EDGE('',*,*,#4588,.T.) ;
#6119 = ORIENTED_EDGE('',*,*,#4585,.F.) ;
#6120 = ORIENTED_EDGE('',*,*,#4402,.F.) ;
#6121 = ORIENTED_EDGE('',*,*,#4589,.T.) ;
#6122 = ORIENTED_EDGE('',*,*,#4590,.T.) ;
#6123 = ORIENTED_EDGE('',*,*,#4587,.F.) ;
#6124 = ORIENTED_EDGE('',*,*,#4401,.F.) ;
#6125 = ORIENTED_EDGE('',*,*,#4591,.T.) ;
#6126 = ORIENTED_EDGE('',*,*,#4592,.T.) ;
#6127 = ORIENTED_EDGE('',*,*,#4589,.F.) ;
#6128 = ORIENTED_EDGE('',*,*,#4400,.F.) ;
#6129 = ORIENTED_EDGE('',*,*,#4593,.T.) ;
#6130 = ORIENTED_EDGE('',*,*,#4594,.T.) ;
#6131 = ORIENTED_EDGE('',*,*,#4591,.F.) ;
#6132 = ORIENTED_EDGE('',*,*,#4399,.F.) ;
#6133 = ORIENTED_EDGE('',*,*,#4595,.T.) ;
#6134 = ORIENTED_EDGE('',*,*,#4596,.T.) ;
#6135 = ORIENTED_EDGE('',*,*,#4593,.F.) ;
#6136 = ORIENTED_EDGE('',*,*,#4398,.F.) ;
#6137 = ORIENTED_EDGE('',*,*,#4597,.T.) ;
#6138 = ORIENTED_EDGE('',*,*,#4598,.T.) ;
#6139 = ORIENTED_EDGE('',*,*,#4595,.F.) ;
#6140 = ORIENTED_EDGE('',*,*,#4397,.F.) ;
#6141 = ORIENTED_EDGE('',*,*,#4599,.T.) ;
#6142 = ORIENTED_EDGE('',*,*,#4600,.T.) ;
#6143 = ORIENTED_EDGE('',*,*,#4597,.F.) ;
#6144 = ORIENTED_EDGE('',*,*,#4396,.F.) ;
#6145 = ORIENTED_EDGE('',*,*,#4601,.T.) ;
#6146 = ORIENTED_EDGE('',*,*,#4602,.T.) ;
#6147 = ORIENTED_EDGE('',*,*,#4599,.F.) ;
#6148 = ORIENTED_EDGE('',*,*,#4395,.F.) ;
#6149 = ORIENTED_EDGE('',*,*,#4603,.T.) ;
#6150 = ORIENTED_EDGE('',*,*,#4604,.T.) ;
#6151 = ORIENTED_EDGE('',*,*,#4601,.F.) ;
#6152 = ORIENTED_EDGE('',*,*,#4394,.F.) ;
#6153 = ORIENTED_EDGE('',*,*,#4605,.T.) ;
#6154 = ORIENTED_EDGE('',*,*,#4606,.T.) ;
#6155 = ORIENTED_EDGE('',*,*,#4603,.F.) ;
#6156 = ORIENTED_EDGE('',*,*,#4393,.F.) ;
#6157 = ORIENTED_EDGE('',*,*,#4607,.T.) ;
#6158 = ORIENTED_EDGE('',*,*,#4608,.T.) ;
#6159 = ORIENTED_EDGE('',*,*,#4605,.F.) ;
#6160 = ORIENTED_EDGE('',*,*,#4392,.F.) ;
#6161 = ORIENTED_EDGE('',*,*,#4609,.T.) ;
#6162 = ORIENTED_EDGE('',*,*,#4610,.T.) ;
#6163 = ORIENTED_EDGE('',*,*,#4607,.F.) ;
#6164 = ORIENTED_EDGE('',*,*,#4391,.F.) ;
#6165 = ORIENTED_EDGE('',*,*,#4611,.T.) ;
#6166 = ORIENTED_EDGE('',*,*,#4612,.T.) ;
#6167 = ORIENTED_EDGE('',*,*,#4609,.F.) ;
#6168 = ORIENTED_EDGE('',*,*,#4390,.F.) ;
#6169 = ORIENTED_EDGE('',*,*,#4580,.T.) ;
#6170 = ORIENTED_EDGE('',*,*,#4613,.T.) ;
#6171 = ORIENTED_EDGE('',*,*,#4611,.F.) ;
#6172 = ORIENTED_EDGE('',*,*,#4613,.F.) ;
#6173 = ORIENTED_EDGE('',*,*,#4579,.F.) ;
#6174 = ORIENTED_EDGE('',*,*,#4577,.F.) ;
#6175 = ORIENTED_EDGE('',*,*,#4575,.F.) ;
#6176 = ORIENTED_EDGE('',*,*,#4573,.F.) ;
#6177 = ORIENTED_EDGE('',*,*,#4571,.F.) ;
#6178 = ORIENTED_EDGE('',*,*,#4569,.F.) ;
#6179 = ORIENTED_EDGE('',*,*,#4567,.F.) ;
#6180 = ORIENTED_EDGE('',*,*,#4565,.F.) ;
#6181 = ORIENTED_EDGE('',*,*,#4563,.F.) ;
#6182 = ORIENTED_EDGE('',*,*,#4561,.F.) ;
#6183 = ORIENTED_EDGE('',*,*,#4559,.F.) ;
#6184 = ORIENTED_EDGE('',*,*,#4557,.F.) ;
#6185 = ORIENTED_EDGE('',*,*,#4555,.F.) ;
#6186 = ORIENTED_EDGE('',*,*,#4553,.F.) ;
#6187 = ORIENTED_EDGE('',*,*,#4551,.F.) ;
#6188 = ORIENTED_EDGE('',*,*,#4549,.F.) ;
#6189 = ORIENTED_EDGE('',*,*,#4547,.F.) ;
#6190 = ORIENTED_EDGE('',*,*,#4545,.F.) ;
#6191 = ORIENTED_EDGE('',*,*,#4582,.F.) ;
#6192 = ORIENTED_EDGE('',*,*,#4584,.F.) ;
#6193 = ORIENTED_EDGE('',*,*,#4586,.F.) ;
#6194 = ORIENTED_EDGE('',*,*,#4588,.F.) ;
#6195 = ORIENTED_EDGE('',*,*,#4590,.F.) ;
#6196 = ORIENTED_EDGE('',*,*,#4592,.F.) ;
#6197 = ORIENTED_EDGE('',*,*,#4594,.F.) ;
#6198 = ORIENTED_EDGE('',*,*,#4596,.F.) ;
#6199 = ORIENTED_EDGE('',*,*,#4598,.F.) ;
#6200 = ORIENTED_EDGE('',*,*,#4600,.F.) ;
#6201 = ORIENTED_EDGE('',*,*,#4602,.F.) ;
#6202 = ORIENTED_EDGE('',*,*,#4604,.F.) ;
#6203 = ORIENTED_EDGE('',*,*,#4606,.F.) ;
#6204 = ORIENTED_EDGE('',*,*,#4608,.F.) ;
#6205 = ORIENTED_EDGE('',*,*,#4610,.F.) ;
#6206 = ORIENTED_EDGE('',*,*,#4612,.F.) ;
#6207 = ORIENTED_EDGE('',*,*,#4382,.F.) ;
#6208 = ORIENTED_EDGE('',*,*,#4614,.T.) ;
#6209 = ORIENTED_EDGE('',*,*,#4615,.T.) ;
#6210 = ORIENTED_EDGE('',*,*,#4616,.F.) ;
#6211 = ORIENTED_EDGE('',*,*,#4383,.F.) ;
#6212 = ORIENTED_EDGE('',*,*,#4616,.T.) ;
#6213 = ORIENTED_EDGE('',*,*,#4617,.T.) ;
#6214 = ORIENTED_EDGE('',*,*,#4618,.F.) ;
#6215 = ORIENTED_EDGE('',*,*,#4384,.F.) ;
#6216 = ORIENTED_EDGE('',*,*,#4618,.T.) ;
#6217 = ORIENTED_EDGE('',*,*,#4619,.T.) ;
#6218 = ORIENTED_EDGE('',*,*,#4620,.F.) ;
#6219 = ORIENTED_EDGE('',*,*,#4385,.F.) ;
#6220 = ORIENTED_EDGE('',*,*,#4620,.T.) ;
#6221 = ORIENTED_EDGE('',*,*,#4621,.T.) ;
#6222 = ORIENTED_EDGE('',*,*,#4622,.F.) ;
#6223 = ORIENTED_EDGE('',*,*,#4386,.F.) ;
#6224 = ORIENTED_EDGE('',*,*,#4622,.T.) ;
#6225 = ORIENTED_EDGE('',*,*,#4623,.T.) ;
#6226 = ORIENTED_EDGE('',*,*,#4624,.F.) ;
#6227 = ORIENTED_EDGE('',*,*,#4387,.F.) ;
#6228 = ORIENTED_EDGE('',*,*,#4624,.T.) ;
#6229 = ORIENTED_EDGE('',*,*,#4625,.T.) ;
#6230 = ORIENTED_EDGE('',*,*,#4626,.F.) ;
#6231 = ORIENTED_EDGE('',*,*,#4388,.F.) ;
#6232 = ORIENTED_EDGE('',*,*,#4626,.T.) ;
#6233 = ORIENTED_EDGE('',*,*,#4627,.T.) ;
#6234 = ORIENTED_EDGE('',*,*,#4628,.F.) ;
#6235 = ORIENTED_EDGE('',*,*,#4374,.F.) ;
#6236 = ORIENTED_EDGE('',*,*,#4628,.T.) ;
#6237 = ORIENTED_EDGE('',*,*,#4629,.T.) ;
#6238 = ORIENTED_EDGE('',*,*,#4630,.F.) ;
#6239 = ORIENTED_EDGE('',*,*,#4381,.F.) ;
#6240 = ORIENTED_EDGE('',*,*,#4631,.T.) ;
#6241 = ORIENTED_EDGE('',*,*,#4632,.T.) ;
#6242 = ORIENTED_EDGE('',*,*,#4614,.F.) ;
#6243 = ORIENTED_EDGE('',*,*,#4380,.F.) ;
#6244 = ORIENTED_EDGE('',*,*,#4633,.T.) ;
#6245 = ORIENTED_EDGE('',*,*,#4634,.T.) ;
#6246 = ORIENTED_EDGE('',*,*,#4631,.F.) ;
#6247 = ORIENTED_EDGE('',*,*,#4379,.F.) ;
#6248 = ORIENTED_EDGE('',*,*,#4635,.T.) ;
#6249 = ORIENTED_EDGE('',*,*,#4636,.T.) ;
#6250 = ORIENTED_EDGE('',*,*,#4633,.F.) ;
#6251 = ORIENTED_EDGE('',*,*,#4378,.F.) ;
#6252 = ORIENTED_EDGE('',*,*,#4637,.T.) ;
#6253 = ORIENTED_EDGE('',*,*,#4638,.T.) ;
#6254 = ORIENTED_EDGE('',*,*,#4635,.F.) ;
#6255 = ORIENTED_EDGE('',*,*,#4377,.F.) ;
#6256 = ORIENTED_EDGE('',*,*,#4639,.T.) ;
#6257 = ORIENTED_EDGE('',*,*,#4640,.T.) ;
#6258 = ORIENTED_EDGE('',*,*,#4637,.F.) ;
#6259 = ORIENTED_EDGE('',*,*,#4376,.F.) ;
#6260 = ORIENTED_EDGE('',*,*,#4641,.T.) ;
#6261 = ORIENTED_EDGE('',*,*,#4642,.T.) ;
#6262 = ORIENTED_EDGE('',*,*,#4639,.F.) ;
#6263 = ORIENTED_EDGE('',*,*,#4375,.F.) ;
#6264 = ORIENTED_EDGE('',*,*,#4630,.T.) ;
#6265 = ORIENTED_EDGE('',*,*,#4643,.T.) ;
#6266 = ORIENTED_EDGE('',*,*,#4641,.F.) ;
#6267 = ORIENTED_EDGE('',*,*,#4643,.F.) ;
#6268 = ORIENTED_EDGE('',*,*,#4629,.F.) ;
#6269 = ORIENTED_EDGE('',*,*,#4627,.F.) ;
#6270 = ORIENTED_EDGE('',*,*,#4625,.F.) ;
#6271 = ORIENTED_EDGE('',*,*,#4623,.F.) ;
#6272 = ORIENTED_EDGE('',*,*,#4621,.F.) ;
#6273 = ORIENTED_EDGE('',*,*,#4619,.F.) ;
#6274 = ORIENTED_EDGE('',*,*,#4617,.F.) ;
#6275 = ORIENTED_EDGE('',*,*,#4615,.F.) ;
#6276 = ORIENTED_EDGE('',*,*,#4632,.F.) ;
#6277 = ORIENTED_EDGE('',*,*,#4634,.F.) ;
#6278 = ORIENTED_EDGE('',*,*,#4636,.F.) ;
#6279 = ORIENTED_EDGE('',*,*,#4638,.F.) ;
#6280 = ORIENTED_EDGE('',*,*,#4640,.F.) ;
#6281 = ORIENTED_EDGE('',*,*,#4642,.F.) ;
#6282 = ORIENTED_EDGE('',*,*,#4644,.T.) ;
#6283 = ORIENTED_EDGE('',*,*,#4645,.T.) ;
#6284 = ORIENTED_EDGE('',*,*,#4646,.F.) ;
#6285 = ORIENTED_EDGE('',*,*,#4645,.F.) ;
#6286 = ORIENTED_EDGE('',*,*,#4647,.F.) ;
#6287 = ORIENTED_EDGE('',*,*,#4644,.F.) ;
#6288 = ORIENTED_EDGE('',*,*,#4373,.F.) ;
#6289 = ORIENTED_EDGE('',*,*,#4646,.T.) ;
#6290 = ORIENTED_EDGE('',*,*,#4301,.T.) ;
#6291 = ORIENTED_EDGE('',*,*,#4313,.T.) ;
#6292 = ORIENTED_EDGE('',*,*,#4310,.T.) ;
#6293 = ORIENTED_EDGE('',*,*,#4307,.T.) ;
#6294 = ORIENTED_EDGE('',*,*,#4304,.T.) ;
#6295 = ORIENTED_EDGE('',*,*,#4260,.T.) ;
#6296 = ORIENTED_EDGE('',*,*,#4264,.T.) ;
#6297 = ORIENTED_EDGE('',*,*,#4267,.T.) ;
#6298 = ORIENTED_EDGE('',*,*,#4270,.T.) ;
#6299 = ORIENTED_EDGE('',*,*,#4648,.T.) ;
#6300 = ORIENTED_EDGE('',*,*,#4649,.T.) ;
#6301 = ORIENTED_EDGE('',*,*,#4650,.T.) ;
#6302 = ORIENTED_EDGE('',*,*,#4651,.T.) ;
#6303 = ORIENTED_EDGE('',*,*,#4652,.T.) ;
#6304 = ORIENTED_EDGE('',*,*,#4648,.F.) ;
#6305 = ORIENTED_EDGE('',*,*,#4653,.T.) ;
#6306 = ORIENTED_EDGE('',*,*,#4651,.F.) ;
#6307 = ORIENTED_EDGE('',*,*,#4654,.T.) ;
#6308 = ORIENTED_EDGE('',*,*,#4653,.F.) ;
#6309 = ORIENTED_EDGE('',*,*,#4655,.T.) ;
#6310 = ORIENTED_EDGE('',*,*,#4656,.F.) ;
#6311 = ORIENTED_EDGE('',*,*,#4657,.T.) ;
#6312 = ORIENTED_EDGE('',*,*,#4658,.F.) ;
#6313 = ORIENTED_EDGE('',*,*,#4659,.T.) ;
#6314 = ORIENTED_EDGE('',*,*,#4660,.F.) ;
#6315 = ORIENTED_EDGE('',*,*,#4661,.T.) ;
#6316 = ORIENTED_EDGE('',*,*,#4662,.T.) ;
#6317 = ORIENTED_EDGE('',*,*,#4663,.T.) ;
#6318 = ORIENTED_EDGE('',*,*,#4664,.T.) ;
#6319 = ORIENTED_EDGE('',*,*,#4662,.F.) ;
#6320 = ORIENTED_EDGE('',*,*,#4665,.T.) ;
#6321 = ORIENTED_EDGE('',*,*,#4649,.F.) ;
#6322 = ORIENTED_EDGE('',*,*,#4654,.F.) ;
#6323 = ORIENTED_EDGE('',*,*,#4650,.F.) ;
#6324 = ORIENTED_EDGE('',*,*,#4666,.T.) ;
#6325 = ORIENTED_EDGE('',*,*,#4667,.T.) ;
#6326 = ORIENTED_EDGE('',*,*,#4666,.F.) ;
#6327 = ORIENTED_EDGE('',*,*,#4668,.T.) ;
#6328 = ORIENTED_EDGE('',*,*,#4669,.T.) ;
#6329 = ORIENTED_EDGE('',*,*,#4670,.T.) ;
#6330 = ORIENTED_EDGE('',*,*,#4671,.T.) ;
#6331 = ORIENTED_EDGE('',*,*,#4672,.T.) ;
#6332 = ORIENTED_EDGE('',*,*,#4668,.F.) ;
#6333 = ORIENTED_EDGE('',*,*,#4660,.T.) ;
#6334 = ORIENTED_EDGE('',*,*,#4671,.F.) ;
#6335 = ORIENTED_EDGE('',*,*,#4673,.T.) ;
#6336 = ORIENTED_EDGE('',*,*,#4669,.F.) ;
#6337 = ORIENTED_EDGE('',*,*,#4673,.F.) ;
#6338 = ORIENTED_EDGE('',*,*,#4670,.F.) ;
#6339 = ORIENTED_EDGE('',*,*,#4674,.T.) ;
#6340 = ORIENTED_EDGE('',*,*,#4675,.T.) ;
#6341 = ORIENTED_EDGE('',*,*,#4674,.F.) ;
#6342 = ORIENTED_EDGE('',*,*,#4676,.T.) ;
#6343 = ORIENTED_EDGE('',*,*,#4677,.T.) ;
#6344 = ORIENTED_EDGE('',*,*,#4678,.T.) ;
#6345 = ORIENTED_EDGE('',*,*,#4679,.T.) ;
#6346 = ORIENTED_EDGE('',*,*,#4680,.T.) ;
#6347 = ORIENTED_EDGE('',*,*,#4676,.F.) ;
#6348 = ORIENTED_EDGE('',*,*,#4658,.T.) ;
#6349 = ORIENTED_EDGE('',*,*,#4679,.F.) ;
#6350 = ORIENTED_EDGE('',*,*,#4681,.T.) ;
#6351 = ORIENTED_EDGE('',*,*,#4677,.F.) ;
#6352 = ORIENTED_EDGE('',*,*,#4681,.F.) ;
#6353 = ORIENTED_EDGE('',*,*,#4678,.F.) ;
#6354 = ORIENTED_EDGE('',*,*,#4682,.T.) ;
#6355 = ORIENTED_EDGE('',*,*,#4683,.T.) ;
#6356 = ORIENTED_EDGE('',*,*,#4682,.F.) ;
#6357 = ORIENTED_EDGE('',*,*,#4684,.T.) ;
#6358 = ORIENTED_EDGE('',*,*,#4685,.T.) ;
#6359 = ORIENTED_EDGE('',*,*,#4686,.T.) ;
#6360 = ORIENTED_EDGE('',*,*,#4687,.T.) ;
#6361 = ORIENTED_EDGE('',*,*,#4688,.T.) ;
#6362 = ORIENTED_EDGE('',*,*,#4684,.F.) ;
#6363 = ORIENTED_EDGE('',*,*,#4656,.T.) ;
#6364 = ORIENTED_EDGE('',*,*,#4687,.F.) ;
#6365 = ORIENTED_EDGE('',*,*,#4689,.T.) ;
#6366 = ORIENTED_EDGE('',*,*,#4685,.F.) ;
#6367 = ORIENTED_EDGE('',*,*,#4689,.F.) ;
#6368 = ORIENTED_EDGE('',*,*,#4686,.F.) ;
#6369 = ORIENTED_EDGE('',*,*,#4690,.T.) ;
#6370 = ORIENTED_EDGE('',*,*,#4691,.T.) ;
#6371 = ORIENTED_EDGE('',*,*,#4690,.F.) ;
#6372 = ORIENTED_EDGE('',*,*,#4691,.F.) ;
#6373 = ORIENTED_EDGE('',*,*,#4692,.F.) ;
#6374 = ORIENTED_EDGE('',*,*,#4683,.F.) ;
#6375 = ORIENTED_EDGE('',*,*,#4693,.F.) ;
#6376 = ORIENTED_EDGE('',*,*,#4675,.F.) ;
#6377 = ORIENTED_EDGE('',*,*,#4694,.F.) ;
#6378 = ORIENTED_EDGE('',*,*,#4667,.F.) ;
#6379 = ORIENTED_EDGE('',*,*,#4695,.F.) ;
#6380 = ORIENTED_EDGE('',*,*,#4692,.T.) ;
#6381 = ORIENTED_EDGE('',*,*,#4696,.T.) ;
#6382 = ORIENTED_EDGE('',*,*,#4697,.F.) ;
#6383 = ORIENTED_EDGE('',*,*,#4696,.F.) ;
#6384 = ORIENTED_EDGE('',*,*,#4693,.T.) ;
#6385 = ORIENTED_EDGE('',*,*,#4698,.T.) ;
#6386 = ORIENTED_EDGE('',*,*,#4699,.F.) ;
#6387 = ORIENTED_EDGE('',*,*,#4698,.F.) ;
#6388 = ORIENTED_EDGE('',*,*,#4694,.T.) ;
#6389 = ORIENTED_EDGE('',*,*,#4700,.T.) ;
#6390 = ORIENTED_EDGE('',*,*,#4701,.F.) ;
#6391 = ORIENTED_EDGE('',*,*,#4700,.F.) ;
#6392 = ORIENTED_EDGE('',*,*,#4695,.T.) ;
#6393 = ORIENTED_EDGE('',*,*,#4702,.T.) ;
#6394 = ORIENTED_EDGE('',*,*,#4703,.F.) ;
#6395 = ORIENTED_EDGE('',*,*,#4702,.F.) ;
#6396 = ORIENTED_EDGE('',*,*,#4704,.F.) ;
#6397 = ORIENTED_EDGE('',*,*,#4705,.F.) ;
#6398 = ORIENTED_EDGE('',*,*,#4706,.F.) ;
#6399 = ORIENTED_EDGE('',*,*,#4707,.F.) ;
#6400 = ORIENTED_EDGE('',*,*,#4708,.F.) ;
#6401 = ORIENTED_EDGE('',*,*,#4709,.F.) ;
#6402 = ORIENTED_EDGE('',*,*,#4710,.F.) ;
#6403 = ORIENTED_EDGE('',*,*,#4711,.F.) ;
#6404 = ORIENTED_EDGE('',*,*,#4712,.F.) ;
#6405 = ORIENTED_EDGE('',*,*,#4713,.F.) ;
#6406 = ORIENTED_EDGE('',*,*,#4714,.F.) ;
#6407 = ORIENTED_EDGE('',*,*,#4715,.F.) ;
#6408 = ORIENTED_EDGE('',*,*,#4716,.F.) ;
#6409 = ORIENTED_EDGE('',*,*,#4717,.F.) ;
#6410 = ORIENTED_EDGE('',*,*,#4718,.F.) ;
#6411 = ORIENTED_EDGE('',*,*,#4719,.F.) ;
#6412 = ORIENTED_EDGE('',*,*,#4720,.T.) ;
#6413 = ORIENTED_EDGE('',*,*,#4707,.T.) ;
#6414 = ORIENTED_EDGE('',*,*,#4721,.F.) ;
#6415 = ORIENTED_EDGE('',*,*,#4717,.T.) ;
#6416 = ORIENTED_EDGE('',*,*,#4722,.F.) ;
#6417 = ORIENTED_EDGE('',*,*,#4713,.T.) ;
#6418 = ORIENTED_EDGE('',*,*,#4723,.F.) ;
#6419 = ORIENTED_EDGE('',*,*,#4711,.T.) ;
#6420 = ORIENTED_EDGE('',*,*,#4724,.F.) ;
#6421 = ORIENTED_EDGE('',*,*,#4714,.T.) ;
#6422 = ORIENTED_EDGE('',*,*,#4722,.T.) ;
#6423 = ORIENTED_EDGE('',*,*,#4716,.T.) ;
#6424 = ORIENTED_EDGE('',*,*,#4725,.F.) ;
#6425 = ORIENTED_EDGE('',*,*,#4708,.T.) ;
#6426 = ORIENTED_EDGE('',*,*,#4723,.T.) ;
#6427 = ORIENTED_EDGE('',*,*,#4712,.T.) ;
#6428 = ORIENTED_EDGE('',*,*,#4726,.F.) ;
#6429 = ORIENTED_EDGE('',*,*,#4706,.T.) ;
#6430 = ORIENTED_EDGE('',*,*,#4727,.F.) ;
#6431 = ORIENTED_EDGE('',*,*,#4718,.T.) ;
#6432 = ORIENTED_EDGE('',*,*,#4721,.T.) ;
#6433 = ORIENTED_EDGE('',*,*,#4704,.T.) ;
#6434 = ORIENTED_EDGE('',*,*,#4724,.T.) ;
#6435 = ORIENTED_EDGE('',*,*,#4710,.T.) ;
#6436 = ORIENTED_EDGE('',*,*,#4728,.F.) ;
#6437 = ORIENTED_EDGE('',*,*,#4729,.T.) ;
#6438 = ORIENTED_EDGE('',*,*,#4652,.F.) ;
#6439 = ORIENTED_EDGE('',*,*,#4665,.F.) ;
#6440 = ORIENTED_EDGE('',*,*,#4661,.F.) ;
#6441 = ORIENTED_EDGE('',*,*,#4672,.F.) ;
#6442 = ORIENTED_EDGE('',*,*,#4659,.F.) ;
#6443 = ORIENTED_EDGE('',*,*,#4680,.F.) ;
#6444 = ORIENTED_EDGE('',*,*,#4657,.F.) ;
#6445 = ORIENTED_EDGE('',*,*,#4688,.F.) ;
#6446 = ORIENTED_EDGE('',*,*,#4655,.F.) ;
#6447 = ORIENTED_EDGE('',*,*,#4647,.T.) ;
#6448 = ORIENTED_EDGE('',*,*,#4730,.T.) ;
#6449 = ORIENTED_EDGE('',*,*,#4663,.F.) ;
#6450 = ORIENTED_EDGE('',*,*,#4664,.F.) ;
#6451 = ORIENTED_EDGE('',*,*,#4730,.F.) ;
#6452 = ORIENTED_EDGE('',*,*,#4731,.T.) ;
#6453 = ORIENTED_EDGE('',*,*,#4732,.F.) ;
#6454 = ORIENTED_EDGE('',*,*,#4731,.F.) ;
#6455 = ORIENTED_EDGE('',*,*,#4733,.T.) ;
#6456 = ORIENTED_EDGE('',*,*,#4734,.T.) ;
#6457 = ORIENTED_EDGE('',*,*,#4733,.F.) ;
#6458 = ORIENTED_EDGE('',*,*,#4734,.F.) ;
#6459 = ORIENTED_EDGE('',*,*,#4735,.F.) ;
#6460 = ORIENTED_EDGE('',*,*,#4736,.T.) ;
#6461 = ORIENTED_EDGE('',*,*,#4737,.T.) ;
#6462 = ORIENTED_EDGE('',*,*,#4735,.T.) ;
#6463 = ORIENTED_EDGE('',*,*,#4737,.F.) ;
#6464 = ORIENTED_EDGE('',*,*,#4738,.T.) ;
#6465 = ORIENTED_EDGE('',*,*,#4739,.F.) ;
#6466 = ORIENTED_EDGE('',*,*,#4738,.F.) ;
#6467 = ORIENTED_EDGE('',*,*,#4740,.T.) ;
#6468 = ORIENTED_EDGE('',*,*,#4741,.T.) ;
#6469 = ORIENTED_EDGE('',*,*,#4740,.F.) ;
#6470 = ORIENTED_EDGE('',*,*,#4741,.F.) ;
#6471 = ORIENTED_EDGE('',*,*,#4742,.F.) ;
#6472 = ORIENTED_EDGE('',*,*,#4743,.T.) ;
#6473 = ORIENTED_EDGE('',*,*,#4744,.T.) ;
#6474 = ORIENTED_EDGE('',*,*,#4742,.T.) ;
#6475 = ORIENTED_EDGE('',*,*,#4744,.F.) ;
#6476 = ORIENTED_EDGE('',*,*,#4743,.F.) ;
#6477 = ORIENTED_EDGE('',*,*,#4705,.T.) ;
#6478 = ORIENTED_EDGE('',*,*,#4728,.T.) ;
#6479 = ORIENTED_EDGE('',*,*,#4709,.T.) ;
#6480 = ORIENTED_EDGE('',*,*,#4726,.T.) ;
#6481 = ORIENTED_EDGE('',*,*,#4715,.T.) ;
#6482 = ORIENTED_EDGE('',*,*,#4725,.T.) ;
#6483 = ORIENTED_EDGE('',*,*,#4719,.T.) ;
#6484 = ORIENTED_EDGE('',*,*,#4727,.T.) ;
#6485 = ORIENTED_EDGE('',*,*,#4739,.T.) ;
#6486 = ORIENTED_EDGE('',*,*,#4745,.T.) ;
#6487 = ORIENTED_EDGE('',*,*,#4746,.F.) ;
#6488 = ORIENTED_EDGE('',*,*,#4745,.F.) ;
#6489 = ORIENTED_EDGE('',*,*,#4747,.F.) ;
#6490 = ORIENTED_EDGE('',*,*,#4746,.T.) ;
#6491 = ORIENTED_EDGE('',*,*,#4703,.T.) ;
#6492 = ORIENTED_EDGE('',*,*,#4701,.T.) ;
#6493 = ORIENTED_EDGE('',*,*,#4699,.T.) ;
#6494 = ORIENTED_EDGE('',*,*,#4697,.T.) ;
#6495 = ORIENTED_EDGE('',*,*,#4748,.F.) ;
#6496 = ORIENTED_EDGE('',*,*,#4749,.T.) ;
#6497 = ORIENTED_EDGE('',*,*,#4747,.T.) ;
#6498 = ORIENTED_EDGE('',*,*,#4749,.F.) ;
#6499 = ORIENTED_EDGE('',*,*,#4750,.F.) ;
#6500 = ORIENTED_EDGE('',*,*,#4751,.T.) ;
#6501 = ORIENTED_EDGE('',*,*,#4748,.T.) ;
#6502 = ORIENTED_EDGE('',*,*,#4751,.F.) ;
#6503 = ORIENTED_EDGE('',*,*,#4729,.F.) ;
#6504 = ORIENTED_EDGE('',*,*,#4752,.T.) ;
#6505 = ORIENTED_EDGE('',*,*,#4750,.T.) ;
#6506 = ORIENTED_EDGE('',*,*,#4752,.F.) ;
#6507 = ORIENTED_EDGE('',*,*,#4753,.F.) ;
#6508 = ORIENTED_EDGE('',*,*,#4754,.T.) ;
#6509 = ORIENTED_EDGE('',*,*,#4371,.T.) ;
#6510 = ORIENTED_EDGE('',*,*,#4754,.F.) ;
#6511 = ORIENTED_EDGE('',*,*,#4753,.T.) ;
#6512 = ORIENTED_EDGE('',*,*,#4736,.F.) ;
#6513 = ORIENTED_EDGE('',*,*,#4732,.T.) ;
#6514 = ORIENTED_EDGE('',*,*,#4755,.T.) ;
#6515 = ORIENTED_EDGE('',*,*,#4720,.F.) ;
#6516 = ORIENTED_EDGE('',*,*,#4755,.F.) ;
#6517 = ORIENTED_EDGE('',*,*,#4756,.F.) ;
#6518 = ORIENTED_EDGE('',*,*,#4757,.T.) ;
#6519 = ORIENTED_EDGE('',*,*,#4758,.F.) ;
#6520 = ORIENTED_EDGE('',*,*,#4759,.T.) ;
#6521 = ORIENTED_EDGE('',*,*,#4760,.F.) ;
#6522 = ORIENTED_EDGE('',*,*,#4759,.F.) ;
#6523 = ORIENTED_EDGE('',*,*,#4761,.F.) ;
#6524 = ORIENTED_EDGE('',*,*,#4762,.F.) ;
#6525 = ORIENTED_EDGE('',*,*,#4763,.F.) ;
#6526 = ORIENTED_EDGE('',*,*,#4762,.T.) ;
#6527 = ORIENTED_EDGE('',*,*,#4764,.F.) ;
#6528 = ORIENTED_EDGE('',*,*,#4765,.T.) ;
#6529 = ORIENTED_EDGE('',*,*,#4766,.F.) ;
#6530 = ORIENTED_EDGE('',*,*,#4765,.F.) ;
#6531 = ORIENTED_EDGE('',*,*,#4767,.F.) ;
#6532 = ORIENTED_EDGE('',*,*,#4757,.F.) ;
#6533 = ORIENTED_EDGE('',*,*,#4768,.F.) ;
#6534 = ORIENTED_EDGE('',*,*,#4769,.T.) ;
#6535 = ORIENTED_EDGE('',*,*,#4770,.F.) ;
#6536 = ORIENTED_EDGE('',*,*,#4771,.T.) ;
#6537 = ORIENTED_EDGE('',*,*,#4772,.F.) ;
#6538 = ORIENTED_EDGE('',*,*,#4771,.F.) ;
#6539 = ORIENTED_EDGE('',*,*,#4773,.F.) ;
#6540 = ORIENTED_EDGE('',*,*,#4774,.F.) ;
#6541 = ORIENTED_EDGE('',*,*,#4775,.F.) ;
#6542 = ORIENTED_EDGE('',*,*,#4774,.T.) ;
#6543 = ORIENTED_EDGE('',*,*,#4776,.F.) ;
#6544 = ORIENTED_EDGE('',*,*,#4777,.T.) ;
#6545 = ORIENTED_EDGE('',*,*,#4778,.F.) ;
#6546 = ORIENTED_EDGE('',*,*,#4777,.F.) ;
#6547 = ORIENTED_EDGE('',*,*,#4779,.F.) ;
#6548 = ORIENTED_EDGE('',*,*,#4769,.F.) ;
#6549 = ORIENTED_EDGE('',*,*,#4780,.F.) ;
#6550 = ORIENTED_EDGE('',*,*,#4781,.T.) ;
#6551 = ORIENTED_EDGE('',*,*,#4782,.F.) ;
#6552 = ORIENTED_EDGE('',*,*,#4783,.T.) ;
#6553 = ORIENTED_EDGE('',*,*,#4784,.F.) ;
#6554 = ORIENTED_EDGE('',*,*,#4783,.F.) ;
#6555 = ORIENTED_EDGE('',*,*,#4785,.F.) ;
#6556 = ORIENTED_EDGE('',*,*,#4786,.F.) ;
#6557 = ORIENTED_EDGE('',*,*,#4787,.F.) ;
#6558 = ORIENTED_EDGE('',*,*,#4786,.T.) ;
#6559 = ORIENTED_EDGE('',*,*,#4788,.F.) ;
#6560 = ORIENTED_EDGE('',*,*,#4789,.T.) ;
#6561 = ORIENTED_EDGE('',*,*,#4790,.F.) ;
#6562 = ORIENTED_EDGE('',*,*,#4789,.F.) ;
#6563 = ORIENTED_EDGE('',*,*,#4791,.F.) ;
#6564 = ORIENTED_EDGE('',*,*,#4781,.F.) ;
#6565 = ORIENTED_EDGE('',*,*,#4792,.F.) ;
#6566 = ORIENTED_EDGE('',*,*,#4793,.T.) ;
#6567 = ORIENTED_EDGE('',*,*,#4794,.F.) ;
#6568 = ORIENTED_EDGE('',*,*,#4795,.T.) ;
#6569 = ORIENTED_EDGE('',*,*,#4796,.F.) ;
#6570 = ORIENTED_EDGE('',*,*,#4795,.F.) ;
#6571 = ORIENTED_EDGE('',*,*,#4797,.F.) ;
#6572 = ORIENTED_EDGE('',*,*,#4798,.F.) ;
#6573 = ORIENTED_EDGE('',*,*,#4799,.F.) ;
#6574 = ORIENTED_EDGE('',*,*,#4798,.T.) ;
#6575 = ORIENTED_EDGE('',*,*,#4800,.F.) ;
#6576 = ORIENTED_EDGE('',*,*,#4801,.T.) ;
#6577 = ORIENTED_EDGE('',*,*,#4802,.F.) ;
#6578 = ORIENTED_EDGE('',*,*,#4801,.F.) ;
#6579 = ORIENTED_EDGE('',*,*,#4803,.F.) ;
#6580 = ORIENTED_EDGE('',*,*,#4793,.F.) ;
#6581 = ORIENTED_EDGE('',*,*,#4804,.T.) ;
#6582 = ORIENTED_EDGE('',*,*,#4805,.T.) ;
#6583 = ORIENTED_EDGE('',*,*,#4806,.F.) ;
#6584 = ORIENTED_EDGE('',*,*,#4805,.F.) ;
#6585 = ORIENTED_EDGE('',*,*,#4763,.T.) ;
#6586 = ORIENTED_EDGE('',*,*,#4766,.T.) ;
#6587 = ORIENTED_EDGE('',*,*,#4756,.T.) ;
#6588 = ORIENTED_EDGE('',*,*,#4760,.T.) ;
#6589 = ORIENTED_EDGE('',*,*,#4775,.T.) ;
#6590 = ORIENTED_EDGE('',*,*,#4778,.T.) ;
#6591 = ORIENTED_EDGE('',*,*,#4768,.T.) ;
#6592 = ORIENTED_EDGE('',*,*,#4772,.T.) ;
#6593 = ORIENTED_EDGE('',*,*,#4787,.T.) ;
#6594 = ORIENTED_EDGE('',*,*,#4790,.T.) ;
#6595 = ORIENTED_EDGE('',*,*,#4780,.T.) ;
#6596 = ORIENTED_EDGE('',*,*,#4784,.T.) ;
#6597 = ORIENTED_EDGE('',*,*,#4799,.T.) ;
#6598 = ORIENTED_EDGE('',*,*,#4802,.T.) ;
#6599 = ORIENTED_EDGE('',*,*,#4792,.T.) ;
#6600 = ORIENTED_EDGE('',*,*,#4796,.T.) ;
#6601 = ORIENTED_EDGE('',*,*,#4807,.F.) ;
#6602 = ORIENTED_EDGE('',*,*,#4806,.T.) ;
#6603 = ORIENTED_EDGE('',*,*,#4808,.F.) ;
#6604 = ORIENTED_EDGE('',*,*,#4809,.T.) ;
#6605 = ORIENTED_EDGE('',*,*,#4807,.T.) ;
#6606 = ORIENTED_EDGE('',*,*,#4809,.F.) ;
#6607 = ORIENTED_EDGE('',*,*,#4764,.T.) ;
#6608 = ORIENTED_EDGE('',*,*,#4761,.T.) ;
#6609 = ORIENTED_EDGE('',*,*,#4758,.T.) ;
#6610 = ORIENTED_EDGE('',*,*,#4767,.T.) ;
#6611 = ORIENTED_EDGE('',*,*,#4776,.T.) ;
#6612 = ORIENTED_EDGE('',*,*,#4773,.T.) ;
#6613 = ORIENTED_EDGE('',*,*,#4770,.T.) ;
#6614 = ORIENTED_EDGE('',*,*,#4779,.T.) ;
#6615 = ORIENTED_EDGE('',*,*,#4788,.T.) ;
#6616 = ORIENTED_EDGE('',*,*,#4785,.T.) ;
#6617 = ORIENTED_EDGE('',*,*,#4782,.T.) ;
#6618 = ORIENTED_EDGE('',*,*,#4791,.T.) ;
#6619 = ORIENTED_EDGE('',*,*,#4800,.T.) ;
#6620 = ORIENTED_EDGE('',*,*,#4797,.T.) ;
#6621 = ORIENTED_EDGE('',*,*,#4794,.T.) ;
#6622 = ORIENTED_EDGE('',*,*,#4803,.T.) ;
#6623 = ORIENTED_EDGE('',*,*,#4808,.T.) ;
#6624 = ORIENTED_EDGE('',*,*,#4804,.F.) ;
#6625 = ORIENTED_EDGE('',*,*,#4810,.T.) ;
#6626 = ORIENTED_EDGE('',*,*,#4810,.F.) ;
#6627 = ORIENTED_EDGE('',*,*,#4811,.F.) ;
#6628 = ORIENTED_EDGE('',*,*,#4812,.T.) ;
#6629 = ORIENTED_EDGE('',*,*,#4813,.F.) ;
#6630 = ORIENTED_EDGE('',*,*,#4814,.T.) ;
#6631 = ORIENTED_EDGE('',*,*,#4815,.F.) ;
#6632 = ORIENTED_EDGE('',*,*,#4816,.T.) ;
#6633 = ORIENTED_EDGE('',*,*,#4811,.T.) ;
#6634 = ORIENTED_EDGE('',*,*,#4817,.T.) ;
#6635 = ORIENTED_EDGE('',*,*,#4818,.F.) ;
#6636 = ORIENTED_EDGE('',*,*,#4819,.T.) ;
#6637 = ORIENTED_EDGE('',*,*,#4815,.T.) ;
#6638 = ORIENTED_EDGE('',*,*,#4820,.T.) ;
#6639 = ORIENTED_EDGE('',*,*,#4821,.F.) ;
#6640 = ORIENTED_EDGE('',*,*,#4822,.T.) ;
#6641 = ORIENTED_EDGE('',*,*,#4818,.T.) ;
#6642 = ORIENTED_EDGE('',*,*,#4823,.T.) ;
#6643 = ORIENTED_EDGE('',*,*,#4824,.F.) ;
#6644 = ORIENTED_EDGE('',*,*,#4825,.T.) ;
#6645 = ORIENTED_EDGE('',*,*,#4821,.T.) ;
#6646 = ORIENTED_EDGE('',*,*,#4826,.T.) ;
#6647 = ORIENTED_EDGE('',*,*,#4827,.F.) ;
#6648 = ORIENTED_EDGE('',*,*,#4828,.T.) ;
#6649 = ORIENTED_EDGE('',*,*,#4824,.T.) ;
#6650 = ORIENTED_EDGE('',*,*,#4829,.T.) ;
#6651 = ORIENTED_EDGE('',*,*,#4830,.F.) ;
#6652 = ORIENTED_EDGE('',*,*,#4831,.T.) ;
#6653 = ORIENTED_EDGE('',*,*,#4827,.T.) ;
#6654 = ORIENTED_EDGE('',*,*,#4832,.T.) ;
#6655 = ORIENTED_EDGE('',*,*,#4833,.F.) ;
#6656 = ORIENTED_EDGE('',*,*,#4834,.T.) ;
#6657 = ORIENTED_EDGE('',*,*,#4830,.T.) ;
#6658 = ORIENTED_EDGE('',*,*,#4835,.T.) ;
#6659 = ORIENTED_EDGE('',*,*,#4836,.F.) ;
#6660 = ORIENTED_EDGE('',*,*,#4837,.T.) ;
#6661 = ORIENTED_EDGE('',*,*,#4833,.T.) ;
#6662 = ORIENTED_EDGE('',*,*,#4838,.T.) ;
#6663 = ORIENTED_EDGE('',*,*,#4839,.F.) ;
#6664 = ORIENTED_EDGE('',*,*,#4840,.T.) ;
#6665 = ORIENTED_EDGE('',*,*,#4836,.T.) ;
#6666 = ORIENTED_EDGE('',*,*,#4841,.T.) ;
#6667 = ORIENTED_EDGE('',*,*,#4842,.F.) ;
#6668 = ORIENTED_EDGE('',*,*,#4843,.T.) ;
#6669 = ORIENTED_EDGE('',*,*,#4839,.T.) ;
#6670 = ORIENTED_EDGE('',*,*,#4844,.T.) ;
#6671 = ORIENTED_EDGE('',*,*,#4845,.F.) ;
#6672 = ORIENTED_EDGE('',*,*,#4846,.T.) ;
#6673 = ORIENTED_EDGE('',*,*,#4842,.T.) ;
#6674 = ORIENTED_EDGE('',*,*,#4847,.T.) ;
#6675 = ORIENTED_EDGE('',*,*,#4848,.F.) ;
#6676 = ORIENTED_EDGE('',*,*,#4849,.T.) ;
#6677 = ORIENTED_EDGE('',*,*,#4845,.T.) ;
#6678 = ORIENTED_EDGE('',*,*,#4850,.T.) ;
#6679 = ORIENTED_EDGE('',*,*,#4851,.F.) ;
#6680 = ORIENTED_EDGE('',*,*,#4852,.F.) ;
#6681 = ORIENTED_EDGE('',*,*,#4853,.T.) ;
#6682 = ORIENTED_EDGE('',*,*,#4848,.T.) ;
#6683 = ORIENTED_EDGE('',*,*,#4854,.T.) ;
#6684 = ORIENTED_EDGE('',*,*,#4855,.F.) ;
#6685 = ORIENTED_EDGE('',*,*,#4856,.T.) ;
#6686 = ORIENTED_EDGE('',*,*,#4857,.F.) ;
#6687 = ORIENTED_EDGE('',*,*,#4858,.F.) ;
#6688 = ORIENTED_EDGE('',*,*,#4859,.F.) ;
#6689 = ORIENTED_EDGE('',*,*,#4860,.T.) ;
#6690 = ORIENTED_EDGE('',*,*,#4855,.T.) ;
#6691 = ORIENTED_EDGE('',*,*,#4861,.F.) ;
#6692 = ORIENTED_EDGE('',*,*,#4862,.F.) ;
#6693 = ORIENTED_EDGE('',*,*,#4863,.T.) ;
#6694 = ORIENTED_EDGE('',*,*,#4859,.T.) ;
#6695 = ORIENTED_EDGE('',*,*,#4864,.F.) ;
#6696 = ORIENTED_EDGE('',*,*,#4865,.F.) ;
#6697 = ORIENTED_EDGE('',*,*,#4866,.T.) ;
#6698 = ORIENTED_EDGE('',*,*,#4862,.T.) ;
#6699 = ORIENTED_EDGE('',*,*,#4867,.F.) ;
#6700 = ORIENTED_EDGE('',*,*,#4868,.F.) ;
#6701 = ORIENTED_EDGE('',*,*,#4869,.T.) ;
#6702 = ORIENTED_EDGE('',*,*,#4865,.T.) ;
#6703 = ORIENTED_EDGE('',*,*,#4870,.F.) ;
#6704 = ORIENTED_EDGE('',*,*,#4871,.F.) ;
#6705 = ORIENTED_EDGE('',*,*,#4872,.T.) ;
#6706 = ORIENTED_EDGE('',*,*,#4868,.T.) ;
#6707 = ORIENTED_EDGE('',*,*,#4873,.F.) ;
#6708 = ORIENTED_EDGE('',*,*,#4874,.F.) ;
#6709 = ORIENTED_EDGE('',*,*,#4875,.T.) ;
#6710 = ORIENTED_EDGE('',*,*,#4871,.T.) ;
#6711 = ORIENTED_EDGE('',*,*,#4876,.F.) ;
#6712 = ORIENTED_EDGE('',*,*,#4877,.F.) ;
#6713 = ORIENTED_EDGE('',*,*,#4878,.T.) ;
#6714 = ORIENTED_EDGE('',*,*,#4874,.T.) ;
#6715 = ORIENTED_EDGE('',*,*,#4879,.F.) ;
#6716 = ORIENTED_EDGE('',*,*,#4880,.F.) ;
#6717 = ORIENTED_EDGE('',*,*,#4881,.T.) ;
#6718 = ORIENTED_EDGE('',*,*,#4877,.T.) ;
#6719 = ORIENTED_EDGE('',*,*,#4882,.F.) ;
#6720 = ORIENTED_EDGE('',*,*,#4883,.F.) ;
#6721 = ORIENTED_EDGE('',*,*,#4884,.T.) ;
#6722 = ORIENTED_EDGE('',*,*,#4880,.T.) ;
#6723 = ORIENTED_EDGE('',*,*,#4885,.F.) ;
#6724 = ORIENTED_EDGE('',*,*,#4886,.F.) ;
#6725 = ORIENTED_EDGE('',*,*,#4887,.T.) ;
#6726 = ORIENTED_EDGE('',*,*,#4883,.T.) ;
#6727 = ORIENTED_EDGE('',*,*,#4888,.F.) ;
#6728 = ORIENTED_EDGE('',*,*,#4889,.F.) ;
#6729 = ORIENTED_EDGE('',*,*,#4890,.T.) ;
#6730 = ORIENTED_EDGE('',*,*,#4886,.T.) ;
#6731 = ORIENTED_EDGE('',*,*,#4891,.F.) ;
#6732 = ORIENTED_EDGE('',*,*,#4892,.F.) ;
#6733 = ORIENTED_EDGE('',*,*,#4893,.T.) ;
#6734 = ORIENTED_EDGE('',*,*,#4889,.T.) ;
#6735 = ORIENTED_EDGE('',*,*,#4894,.F.) ;
#6736 = ORIENTED_EDGE('',*,*,#4857,.T.) ;
#6737 = ORIENTED_EDGE('',*,*,#4895,.T.) ;
#6738 = ORIENTED_EDGE('',*,*,#4896,.F.) ;
#6739 = ORIENTED_EDGE('',*,*,#4897,.T.) ;
#6740 = ORIENTED_EDGE('',*,*,#4897,.F.) ;
#6741 = ORIENTED_EDGE('',*,*,#4898,.F.) ;
#6742 = ORIENTED_EDGE('',*,*,#4854,.F.) ;
#6743 = ORIENTED_EDGE('',*,*,#4850,.F.) ;
#6744 = ORIENTED_EDGE('',*,*,#4847,.F.) ;
#6745 = ORIENTED_EDGE('',*,*,#4844,.F.) ;
#6746 = ORIENTED_EDGE('',*,*,#4841,.F.) ;
#6747 = ORIENTED_EDGE('',*,*,#4838,.F.) ;
#6748 = ORIENTED_EDGE('',*,*,#4835,.F.) ;
#6749 = ORIENTED_EDGE('',*,*,#4832,.F.) ;
#6750 = ORIENTED_EDGE('',*,*,#4829,.F.) ;
#6751 = ORIENTED_EDGE('',*,*,#4826,.F.) ;
#6752 = ORIENTED_EDGE('',*,*,#4823,.F.) ;
#6753 = ORIENTED_EDGE('',*,*,#4820,.F.) ;
#6754 = ORIENTED_EDGE('',*,*,#4817,.F.) ;
#6755 = ORIENTED_EDGE('',*,*,#4814,.F.) ;
#6756 = ORIENTED_EDGE('',*,*,#4899,.F.) ;
#6757 = ORIENTED_EDGE('',*,*,#4900,.T.) ;
#6758 = ORIENTED_EDGE('',*,*,#4894,.T.) ;
#6759 = ORIENTED_EDGE('',*,*,#4891,.T.) ;
#6760 = ORIENTED_EDGE('',*,*,#4888,.T.) ;
#6761 = ORIENTED_EDGE('',*,*,#4885,.T.) ;
#6762 = ORIENTED_EDGE('',*,*,#4882,.T.) ;
#6763 = ORIENTED_EDGE('',*,*,#4879,.T.) ;
#6764 = ORIENTED_EDGE('',*,*,#4876,.T.) ;
#6765 = ORIENTED_EDGE('',*,*,#4873,.T.) ;
#6766 = ORIENTED_EDGE('',*,*,#4870,.T.) ;
#6767 = ORIENTED_EDGE('',*,*,#4867,.T.) ;
#6768 = ORIENTED_EDGE('',*,*,#4864,.T.) ;
#6769 = ORIENTED_EDGE('',*,*,#4861,.T.) ;
#6770 = ORIENTED_EDGE('',*,*,#4858,.T.) ;
#6771 = ORIENTED_EDGE('',*,*,#4901,.F.) ;
#6772 = ORIENTED_EDGE('',*,*,#4902,.T.) ;
#6773 = ORIENTED_EDGE('',*,*,#4903,.T.) ;
#6774 = ORIENTED_EDGE('',*,*,#4899,.T.) ;
#6775 = ORIENTED_EDGE('',*,*,#4904,.F.) ;
#6776 = ORIENTED_EDGE('',*,*,#4892,.T.) ;
#6777 = ORIENTED_EDGE('',*,*,#4900,.F.) ;
#6778 = ORIENTED_EDGE('',*,*,#4903,.F.) ;
#6779 = ORIENTED_EDGE('',*,*,#4905,.T.) ;
#6780 = ORIENTED_EDGE('',*,*,#4895,.F.) ;
#6781 = ORIENTED_EDGE('',*,*,#4856,.F.) ;
#6782 = ORIENTED_EDGE('',*,*,#4860,.F.) ;
#6783 = ORIENTED_EDGE('',*,*,#4863,.F.) ;
#6784 = ORIENTED_EDGE('',*,*,#4866,.F.) ;
#6785 = ORIENTED_EDGE('',*,*,#4869,.F.) ;
#6786 = ORIENTED_EDGE('',*,*,#4872,.F.) ;
#6787 = ORIENTED_EDGE('',*,*,#4875,.F.) ;
#6788 = ORIENTED_EDGE('',*,*,#4878,.F.) ;
#6789 = ORIENTED_EDGE('',*,*,#4881,.F.) ;
#6790 = ORIENTED_EDGE('',*,*,#4884,.F.) ;
#6791 = ORIENTED_EDGE('',*,*,#4887,.F.) ;
#6792 = ORIENTED_EDGE('',*,*,#4890,.F.) ;
#6793 = ORIENTED_EDGE('',*,*,#4893,.F.) ;
#6794 = ORIENTED_EDGE('',*,*,#4905,.F.) ;
#6795 = ORIENTED_EDGE('',*,*,#4902,.F.) ;
#6796 = ORIENTED_EDGE('',*,*,#4812,.F.) ;
#6797 = ORIENTED_EDGE('',*,*,#4816,.F.) ;
#6798 = ORIENTED_EDGE('',*,*,#4819,.F.) ;
#6799 = ORIENTED_EDGE('',*,*,#4822,.F.) ;
#6800 = ORIENTED_EDGE('',*,*,#4825,.F.) ;
#6801 = ORIENTED_EDGE('',*,*,#4828,.F.) ;
#6802 = ORIENTED_EDGE('',*,*,#4831,.F.) ;
#6803 = ORIENTED_EDGE('',*,*,#4834,.F.) ;
#6804 = ORIENTED_EDGE('',*,*,#4837,.F.) ;
#6805 = ORIENTED_EDGE('',*,*,#4840,.F.) ;
#6806 = ORIENTED_EDGE('',*,*,#4843,.F.) ;
#6807 = ORIENTED_EDGE('',*,*,#4846,.F.) ;
#6808 = ORIENTED_EDGE('',*,*,#4849,.F.) ;
#6809 = ORIENTED_EDGE('',*,*,#4853,.F.) ;
#6810 = ORIENTED_EDGE('',*,*,#4901,.T.) ;
#6811 = ORIENTED_EDGE('',*,*,#4906,.T.) ;
#6812 = ORIENTED_EDGE('',*,*,#4907,.T.) ;
#6813 = ORIENTED_EDGE('',*,*,#4906,.F.) ;
#6814 = ORIENTED_EDGE('',*,*,#4904,.T.) ;
#6815 = ORIENTED_EDGE('',*,*,#4813,.T.) ;
#6816 = ORIENTED_EDGE('',*,*,#4851,.T.) ;
#6817 = ORIENTED_EDGE('',*,*,#4898,.T.) ;
#6818 = ORIENTED_EDGE('',*,*,#4908,.F.) ;
#6819 = ORIENTED_EDGE('',*,*,#4909,.F.) ;
#6820 = ORIENTED_EDGE('',*,*,#4907,.F.) ;
#6821 = ORIENTED_EDGE('',*,*,#4852,.T.) ;
#6822 = ORIENTED_EDGE('',*,*,#4910,.T.) ;
#6823 = ORIENTED_EDGE('',*,*,#4911,.T.) ;
#6824 = ORIENTED_EDGE('',*,*,#4910,.F.) ;
#6825 = ORIENTED_EDGE('',*,*,#4908,.T.) ;
#6826 = ORIENTED_EDGE('',*,*,#4896,.T.) ;
#6827 = ORIENTED_EDGE('',*,*,#4911,.F.) ;
#6828 = ORIENTED_EDGE('',*,*,#4912,.F.) ;
#6829 = ORIENTED_EDGE('',*,*,#4913,.T.) ;
#6830 = ORIENTED_EDGE('',*,*,#4914,.T.) ;
#6831 = ORIENTED_EDGE('',*,*,#4915,.F.) ;
#6832 = ORIENTED_EDGE('',*,*,#4916,.F.) ;
#6833 = ORIENTED_EDGE('',*,*,#4914,.F.) ;
#6834 = ORIENTED_EDGE('',*,*,#4917,.F.) ;
#6835 = ORIENTED_EDGE('',*,*,#4918,.F.) ;
#6836 = ORIENTED_EDGE('',*,*,#4919,.F.) ;
#6837 = ORIENTED_EDGE('',*,*,#4917,.T.) ;
#6838 = ORIENTED_EDGE('',*,*,#4913,.F.) ;
#6839 = ORIENTED_EDGE('',*,*,#4915,.T.) ;
#6840 = ORIENTED_EDGE('',*,*,#4916,.T.) ;
#6841 = ORIENTED_EDGE('',*,*,#4919,.T.) ;
#6842 = ORIENTED_EDGE('',*,*,#4920,.F.) ;
#6843 = ORIENTED_EDGE('',*,*,#4921,.T.) ;
#6844 = ORIENTED_EDGE('',*,*,#4922,.T.) ;
#6845 = ORIENTED_EDGE('',*,*,#4923,.T.) ;
#6846 = ORIENTED_EDGE('',*,*,#4924,.F.) ;
#6847 = ORIENTED_EDGE('',*,*,#4925,.T.) ;
#6848 = ORIENTED_EDGE('',*,*,#4926,.T.) ;
#6849 = ORIENTED_EDGE('',*,*,#4927,.T.) ;
#6850 = ORIENTED_EDGE('',*,*,#4928,.F.) ;
#6851 = ORIENTED_EDGE('',*,*,#4929,.T.) ;
#6852 = ORIENTED_EDGE('',*,*,#4930,.T.) ;
#6853 = ORIENTED_EDGE('',*,*,#4931,.T.) ;
#6854 = ORIENTED_EDGE('',*,*,#4932,.F.) ;
#6855 = ORIENTED_EDGE('',*,*,#4933,.T.) ;
#6856 = ORIENTED_EDGE('',*,*,#4934,.T.) ;
#6857 = ORIENTED_EDGE('',*,*,#4935,.T.) ;
#6858 = ORIENTED_EDGE('',*,*,#4936,.F.) ;
#6859 = ORIENTED_EDGE('',*,*,#4937,.T.) ;
#6860 = ORIENTED_EDGE('',*,*,#4938,.T.) ;
#6861 = ORIENTED_EDGE('',*,*,#4939,.T.) ;
#6862 = ORIENTED_EDGE('',*,*,#4940,.F.) ;
#6863 = ORIENTED_EDGE('',*,*,#4941,.T.) ;
#6864 = ORIENTED_EDGE('',*,*,#4942,.T.) ;
#6865 = ORIENTED_EDGE('',*,*,#4943,.T.) ;
#6866 = ORIENTED_EDGE('',*,*,#4944,.F.) ;
#6867 = ORIENTED_EDGE('',*,*,#4945,.T.) ;
#6868 = ORIENTED_EDGE('',*,*,#4946,.T.) ;
#6869 = ORIENTED_EDGE('',*,*,#4947,.T.) ;
#6870 = ORIENTED_EDGE('',*,*,#4948,.F.) ;
#6871 = ORIENTED_EDGE('',*,*,#4949,.T.) ;
#6872 = ORIENTED_EDGE('',*,*,#4950,.T.) ;
#6873 = ORIENTED_EDGE('',*,*,#4951,.T.) ;
#6874 = ORIENTED_EDGE('',*,*,#4952,.F.) ;
#6875 = ORIENTED_EDGE('',*,*,#4953,.T.) ;
#6876 = ORIENTED_EDGE('',*,*,#4954,.T.) ;
#6877 = ORIENTED_EDGE('',*,*,#4955,.T.) ;
#6878 = ORIENTED_EDGE('',*,*,#4956,.F.) ;
#6879 = ORIENTED_EDGE('',*,*,#4957,.T.) ;
#6880 = ORIENTED_EDGE('',*,*,#4958,.T.) ;
#6881 = ORIENTED_EDGE('',*,*,#4959,.T.) ;
#6882 = ORIENTED_EDGE('',*,*,#4960,.F.) ;
#6883 = ORIENTED_EDGE('',*,*,#4961,.T.) ;
#6884 = ORIENTED_EDGE('',*,*,#4962,.T.) ;
#6885 = ORIENTED_EDGE('',*,*,#4963,.T.) ;
#6886 = ORIENTED_EDGE('',*,*,#4964,.F.) ;
#6887 = ORIENTED_EDGE('',*,*,#4965,.T.) ;
#6888 = ORIENTED_EDGE('',*,*,#4966,.T.) ;
#6889 = ORIENTED_EDGE('',*,*,#4967,.T.) ;
#6890 = ORIENTED_EDGE('',*,*,#4968,.F.) ;
#6891 = ORIENTED_EDGE('',*,*,#4969,.T.) ;
#6892 = ORIENTED_EDGE('',*,*,#4970,.T.) ;
#6893 = ORIENTED_EDGE('',*,*,#4971,.T.) ;
#6894 = ORIENTED_EDGE('',*,*,#4972,.F.) ;
#6895 = ORIENTED_EDGE('',*,*,#4973,.T.) ;
#6896 = ORIENTED_EDGE('',*,*,#4974,.T.) ;
#6897 = ORIENTED_EDGE('',*,*,#4975,.T.) ;
#6898 = ORIENTED_EDGE('',*,*,#4976,.F.) ;
#6899 = ORIENTED_EDGE('',*,*,#4977,.T.) ;
#6900 = ORIENTED_EDGE('',*,*,#4978,.T.) ;
#6901 = ORIENTED_EDGE('',*,*,#4979,.T.) ;
#6902 = ORIENTED_EDGE('',*,*,#4980,.F.) ;
#6903 = ORIENTED_EDGE('',*,*,#4981,.T.) ;
#6904 = ORIENTED_EDGE('',*,*,#4982,.T.) ;
#6905 = ORIENTED_EDGE('',*,*,#4983,.T.) ;
#6906 = ORIENTED_EDGE('',*,*,#4984,.F.) ;
#6907 = ORIENTED_EDGE('',*,*,#4985,.T.) ;
#6908 = ORIENTED_EDGE('',*,*,#4986,.T.) ;
#6909 = ORIENTED_EDGE('',*,*,#4987,.T.) ;
#6910 = ORIENTED_EDGE('',*,*,#4988,.F.) ;
#6911 = ORIENTED_EDGE('',*,*,#4989,.T.) ;
#6912 = ORIENTED_EDGE('',*,*,#4990,.T.) ;
#6913 = ORIENTED_EDGE('',*,*,#4991,.T.) ;
#6914 = ORIENTED_EDGE('',*,*,#4992,.F.) ;
#6915 = ORIENTED_EDGE('',*,*,#4993,.T.) ;
#6916 = ORIENTED_EDGE('',*,*,#4994,.T.) ;
#6917 = ORIENTED_EDGE('',*,*,#4995,.T.) ;
#6918 = ORIENTED_EDGE('',*,*,#4996,.F.) ;
#6919 = ORIENTED_EDGE('',*,*,#4997,.T.) ;
#6920 = ORIENTED_EDGE('',*,*,#4998,.T.) ;
#6921 = ORIENTED_EDGE('',*,*,#4999,.T.) ;
#6922 = ORIENTED_EDGE('',*,*,#5000,.F.) ;
#6923 = ORIENTED_EDGE('',*,*,#5001,.T.) ;
#6924 = ORIENTED_EDGE('',*,*,#5002,.T.) ;
#6925 = ORIENTED_EDGE('',*,*,#5003,.T.) ;
#6926 = ORIENTED_EDGE('',*,*,#5004,.F.) ;
#6927 = ORIENTED_EDGE('',*,*,#5005,.T.) ;
#6928 = ORIENTED_EDGE('',*,*,#5006,.T.) ;
#6929 = ORIENTED_EDGE('',*,*,#5007,.T.) ;
#6930 = ORIENTED_EDGE('',*,*,#5008,.F.) ;
#6931 = ORIENTED_EDGE('',*,*,#5009,.T.) ;
#6932 = ORIENTED_EDGE('',*,*,#5010,.T.) ;
#6933 = ORIENTED_EDGE('',*,*,#5011,.T.) ;
#6934 = ORIENTED_EDGE('',*,*,#5012,.F.) ;
#6935 = ORIENTED_EDGE('',*,*,#5013,.T.) ;
#6936 = ORIENTED_EDGE('',*,*,#5014,.T.) ;
#6937 = ORIENTED_EDGE('',*,*,#5015,.T.) ;
#6938 = ORIENTED_EDGE('',*,*,#5016,.F.) ;
#6939 = ORIENTED_EDGE('',*,*,#5017,.T.) ;
#6940 = ORIENTED_EDGE('',*,*,#5018,.T.) ;
#6941 = ORIENTED_EDGE('',*,*,#5019,.T.) ;
#6942 = ORIENTED_EDGE('',*,*,#5020,.F.) ;
#6943 = ORIENTED_EDGE('',*,*,#5021,.T.) ;
#6944 = ORIENTED_EDGE('',*,*,#5022,.T.) ;
#6945 = ORIENTED_EDGE('',*,*,#5023,.T.) ;
#6946 = ORIENTED_EDGE('',*,*,#5024,.F.) ;
#6947 = ORIENTED_EDGE('',*,*,#5025,.T.) ;
#6948 = ORIENTED_EDGE('',*,*,#5026,.T.) ;
#6949 = ORIENTED_EDGE('',*,*,#5027,.T.) ;
#6950 = ORIENTED_EDGE('',*,*,#5028,.F.) ;
#6951 = ORIENTED_EDGE('',*,*,#5029,.T.) ;
#6952 = ORIENTED_EDGE('',*,*,#5030,.T.) ;
#6953 = ORIENTED_EDGE('',*,*,#5031,.T.) ;
#6954 = ORIENTED_EDGE('',*,*,#5032,.F.) ;
#6955 = ORIENTED_EDGE('',*,*,#5031,.F.) ;
#6956 = ORIENTED_EDGE('',*,*,#5033,.T.) ;
#6957 = ORIENTED_EDGE('',*,*,#5034,.T.) ;
#6958 = ORIENTED_EDGE('',*,*,#5035,.F.) ;
#6959 = ORIENTED_EDGE('',*,*,#5036,.T.) ;
#6960 = ORIENTED_EDGE('',*,*,#5037,.T.) ;
#6961 = ORIENTED_EDGE('',*,*,#5038,.T.) ;
#6962 = ORIENTED_EDGE('',*,*,#5039,.F.) ;
#6963 = ORIENTED_EDGE('',*,*,#5040,.T.) ;
#6964 = ORIENTED_EDGE('',*,*,#5041,.T.) ;
#6965 = ORIENTED_EDGE('',*,*,#5042,.T.) ;
#6966 = ORIENTED_EDGE('',*,*,#5043,.F.) ;
#6967 = ORIENTED_EDGE('',*,*,#5044,.T.) ;
#6968 = ORIENTED_EDGE('',*,*,#5045,.T.) ;
#6969 = ORIENTED_EDGE('',*,*,#5046,.T.) ;
#6970 = ORIENTED_EDGE('',*,*,#5047,.F.) ;
#6971 = ORIENTED_EDGE('',*,*,#5048,.T.) ;
#6972 = ORIENTED_EDGE('',*,*,#5049,.T.) ;
#6973 = ORIENTED_EDGE('',*,*,#5050,.T.) ;
#6974 = ORIENTED_EDGE('',*,*,#5051,.F.) ;
#6975 = ORIENTED_EDGE('',*,*,#5052,.T.) ;
#6976 = ORIENTED_EDGE('',*,*,#5053,.T.) ;
#6977 = ORIENTED_EDGE('',*,*,#5054,.T.) ;
#6978 = ORIENTED_EDGE('',*,*,#5055,.F.) ;
#6979 = ORIENTED_EDGE('',*,*,#5056,.T.) ;
#6980 = ORIENTED_EDGE('',*,*,#5057,.T.) ;
#6981 = ORIENTED_EDGE('',*,*,#5058,.T.) ;
#6982 = ORIENTED_EDGE('',*,*,#5059,.F.) ;
#6983 = ORIENTED_EDGE('',*,*,#5060,.T.) ;
#6984 = ORIENTED_EDGE('',*,*,#5061,.T.) ;
#6985 = ORIENTED_EDGE('',*,*,#5062,.T.) ;
#6986 = ORIENTED_EDGE('',*,*,#5063,.F.) ;
#6987 = ORIENTED_EDGE('',*,*,#5064,.F.) ;
#6988 = ORIENTED_EDGE('',*,*,#5065,.T.) ;
#6989 = ORIENTED_EDGE('',*,*,#5066,.T.) ;
#6990 = ORIENTED_EDGE('',*,*,#5060,.F.) ;
#6991 = ORIENTED_EDGE('',*,*,#5061,.F.) ;
#6992 = ORIENTED_EDGE('',*,*,#5066,.F.) ;
#6993 = ORIENTED_EDGE('',*,*,#5067,.F.) ;
#6994 = ORIENTED_EDGE('',*,*,#5068,.F.) ;
#6995 = ORIENTED_EDGE('',*,*,#5062,.F.) ;
#6996 = ORIENTED_EDGE('',*,*,#5067,.T.) ;
#6997 = ORIENTED_EDGE('',*,*,#5065,.F.) ;
#6998 = ORIENTED_EDGE('',*,*,#5069,.F.) ;
#6999 = ORIENTED_EDGE('',*,*,#5070,.T.) ;
#7000 = ORIENTED_EDGE('',*,*,#5071,.T.) ;
#7001 = ORIENTED_EDGE('',*,*,#5056,.F.) ;
#7002 = ORIENTED_EDGE('',*,*,#5057,.F.) ;
#7003 = ORIENTED_EDGE('',*,*,#5071,.F.) ;
#7004 = ORIENTED_EDGE('',*,*,#5072,.F.) ;
#7005 = ORIENTED_EDGE('',*,*,#5073,.F.) ;
#7006 = ORIENTED_EDGE('',*,*,#5058,.F.) ;
#7007 = ORIENTED_EDGE('',*,*,#5072,.T.) ;
#7008 = ORIENTED_EDGE('',*,*,#5070,.F.) ;
#7009 = ORIENTED_EDGE('',*,*,#5074,.F.) ;
#7010 = ORIENTED_EDGE('',*,*,#5075,.T.) ;
#7011 = ORIENTED_EDGE('',*,*,#5076,.T.) ;
#7012 = ORIENTED_EDGE('',*,*,#5052,.F.) ;
#7013 = ORIENTED_EDGE('',*,*,#5053,.F.) ;
#7014 = ORIENTED_EDGE('',*,*,#5076,.F.) ;
#7015 = ORIENTED_EDGE('',*,*,#5077,.F.) ;
#7016 = ORIENTED_EDGE('',*,*,#5078,.F.) ;
#7017 = ORIENTED_EDGE('',*,*,#5054,.F.) ;
#7018 = ORIENTED_EDGE('',*,*,#5077,.T.) ;
#7019 = ORIENTED_EDGE('',*,*,#5075,.F.) ;
#7020 = ORIENTED_EDGE('',*,*,#5079,.F.) ;
#7021 = ORIENTED_EDGE('',*,*,#5080,.T.) ;
#7022 = ORIENTED_EDGE('',*,*,#5081,.T.) ;
#7023 = ORIENTED_EDGE('',*,*,#5048,.F.) ;
#7024 = ORIENTED_EDGE('',*,*,#5049,.F.) ;
#7025 = ORIENTED_EDGE('',*,*,#5081,.F.) ;
#7026 = ORIENTED_EDGE('',*,*,#5082,.F.) ;
#7027 = ORIENTED_EDGE('',*,*,#5083,.F.) ;
#7028 = ORIENTED_EDGE('',*,*,#5050,.F.) ;
#7029 = ORIENTED_EDGE('',*,*,#5082,.T.) ;
#7030 = ORIENTED_EDGE('',*,*,#5080,.F.) ;
#7031 = ORIENTED_EDGE('',*,*,#5084,.F.) ;
#7032 = ORIENTED_EDGE('',*,*,#5085,.T.) ;
#7033 = ORIENTED_EDGE('',*,*,#5086,.T.) ;
#7034 = ORIENTED_EDGE('',*,*,#5044,.F.) ;
#7035 = ORIENTED_EDGE('',*,*,#5045,.F.) ;
#7036 = ORIENTED_EDGE('',*,*,#5086,.F.) ;
#7037 = ORIENTED_EDGE('',*,*,#5087,.F.) ;
#7038 = ORIENTED_EDGE('',*,*,#5088,.F.) ;
#7039 = ORIENTED_EDGE('',*,*,#5046,.F.) ;
#7040 = ORIENTED_EDGE('',*,*,#5087,.T.) ;
#7041 = ORIENTED_EDGE('',*,*,#5085,.F.) ;
#7042 = ORIENTED_EDGE('',*,*,#5089,.F.) ;
#7043 = ORIENTED_EDGE('',*,*,#5090,.T.) ;
#7044 = ORIENTED_EDGE('',*,*,#5091,.T.) ;
#7045 = ORIENTED_EDGE('',*,*,#5040,.F.) ;
#7046 = ORIENTED_EDGE('',*,*,#5041,.F.) ;
#7047 = ORIENTED_EDGE('',*,*,#5091,.F.) ;
#7048 = ORIENTED_EDGE('',*,*,#5092,.F.) ;
#7049 = ORIENTED_EDGE('',*,*,#5093,.F.) ;
#7050 = ORIENTED_EDGE('',*,*,#5042,.F.) ;
#7051 = ORIENTED_EDGE('',*,*,#5092,.T.) ;
#7052 = ORIENTED_EDGE('',*,*,#5090,.F.) ;
#7053 = ORIENTED_EDGE('',*,*,#5094,.F.) ;
#7054 = ORIENTED_EDGE('',*,*,#5095,.T.) ;
#7055 = ORIENTED_EDGE('',*,*,#5096,.T.) ;
#7056 = ORIENTED_EDGE('',*,*,#5036,.F.) ;
#7057 = ORIENTED_EDGE('',*,*,#5037,.F.) ;
#7058 = ORIENTED_EDGE('',*,*,#5096,.F.) ;
#7059 = ORIENTED_EDGE('',*,*,#5097,.F.) ;
#7060 = ORIENTED_EDGE('',*,*,#5098,.F.) ;
#7061 = ORIENTED_EDGE('',*,*,#5038,.F.) ;
#7062 = ORIENTED_EDGE('',*,*,#5097,.T.) ;
#7063 = ORIENTED_EDGE('',*,*,#5095,.F.) ;
#7064 = ORIENTED_EDGE('',*,*,#5099,.F.) ;
#7065 = ORIENTED_EDGE('',*,*,#5100,.T.) ;
#7066 = ORIENTED_EDGE('',*,*,#5101,.T.) ;
#7067 = ORIENTED_EDGE('',*,*,#5029,.F.) ;
#7068 = ORIENTED_EDGE('',*,*,#5030,.F.) ;
#7069 = ORIENTED_EDGE('',*,*,#5101,.F.) ;
#7070 = ORIENTED_EDGE('',*,*,#5102,.F.) ;
#7071 = ORIENTED_EDGE('',*,*,#5033,.F.) ;
#7072 = ORIENTED_EDGE('',*,*,#5103,.F.) ;
#7073 = ORIENTED_EDGE('',*,*,#5034,.F.) ;
#7074 = ORIENTED_EDGE('',*,*,#5102,.T.) ;
#7075 = ORIENTED_EDGE('',*,*,#5100,.F.) ;
#7076 = ORIENTED_EDGE('',*,*,#5104,.F.) ;
#7077 = ORIENTED_EDGE('',*,*,#5105,.T.) ;
#7078 = ORIENTED_EDGE('',*,*,#5106,.T.) ;
#7079 = ORIENTED_EDGE('',*,*,#5025,.F.) ;
#7080 = ORIENTED_EDGE('',*,*,#5026,.F.) ;
#7081 = ORIENTED_EDGE('',*,*,#5106,.F.) ;
#7082 = ORIENTED_EDGE('',*,*,#5107,.F.) ;
#7083 = ORIENTED_EDGE('',*,*,#5108,.F.) ;
#7084 = ORIENTED_EDGE('',*,*,#5027,.F.) ;
#7085 = ORIENTED_EDGE('',*,*,#5107,.T.) ;
#7086 = ORIENTED_EDGE('',*,*,#5105,.F.) ;
#7087 = ORIENTED_EDGE('',*,*,#5109,.F.) ;
#7088 = ORIENTED_EDGE('',*,*,#5110,.T.) ;
#7089 = ORIENTED_EDGE('',*,*,#5111,.T.) ;
#7090 = ORIENTED_EDGE('',*,*,#5021,.F.) ;
#7091 = ORIENTED_EDGE('',*,*,#5022,.F.) ;
#7092 = ORIENTED_EDGE('',*,*,#5111,.F.) ;
#7093 = ORIENTED_EDGE('',*,*,#5112,.F.) ;
#7094 = ORIENTED_EDGE('',*,*,#5113,.F.) ;
#7095 = ORIENTED_EDGE('',*,*,#5023,.F.) ;
#7096 = ORIENTED_EDGE('',*,*,#5112,.T.) ;
#7097 = ORIENTED_EDGE('',*,*,#5110,.F.) ;
#7098 = ORIENTED_EDGE('',*,*,#5114,.F.) ;
#7099 = ORIENTED_EDGE('',*,*,#5115,.T.) ;
#7100 = ORIENTED_EDGE('',*,*,#5116,.T.) ;
#7101 = ORIENTED_EDGE('',*,*,#5017,.F.) ;
#7102 = ORIENTED_EDGE('',*,*,#5018,.F.) ;
#7103 = ORIENTED_EDGE('',*,*,#5116,.F.) ;
#7104 = ORIENTED_EDGE('',*,*,#5117,.F.) ;
#7105 = ORIENTED_EDGE('',*,*,#5118,.F.) ;
#7106 = ORIENTED_EDGE('',*,*,#5019,.F.) ;
#7107 = ORIENTED_EDGE('',*,*,#5117,.T.) ;
#7108 = ORIENTED_EDGE('',*,*,#5115,.F.) ;
#7109 = ORIENTED_EDGE('',*,*,#5119,.F.) ;
#7110 = ORIENTED_EDGE('',*,*,#5120,.T.) ;
#7111 = ORIENTED_EDGE('',*,*,#5121,.T.) ;
#7112 = ORIENTED_EDGE('',*,*,#5013,.F.) ;
#7113 = ORIENTED_EDGE('',*,*,#5014,.F.) ;
#7114 = ORIENTED_EDGE('',*,*,#5121,.F.) ;
#7115 = ORIENTED_EDGE('',*,*,#5122,.F.) ;
#7116 = ORIENTED_EDGE('',*,*,#5123,.F.) ;
#7117 = ORIENTED_EDGE('',*,*,#5015,.F.) ;
#7118 = ORIENTED_EDGE('',*,*,#5122,.T.) ;
#7119 = ORIENTED_EDGE('',*,*,#5120,.F.) ;
#7120 = ORIENTED_EDGE('',*,*,#5124,.F.) ;
#7121 = ORIENTED_EDGE('',*,*,#5125,.T.) ;
#7122 = ORIENTED_EDGE('',*,*,#5126,.T.) ;
#7123 = ORIENTED_EDGE('',*,*,#5009,.F.) ;
#7124 = ORIENTED_EDGE('',*,*,#5010,.F.) ;
#7125 = ORIENTED_EDGE('',*,*,#5126,.F.) ;
#7126 = ORIENTED_EDGE('',*,*,#5127,.F.) ;
#7127 = ORIENTED_EDGE('',*,*,#5128,.F.) ;
#7128 = ORIENTED_EDGE('',*,*,#5011,.F.) ;
#7129 = ORIENTED_EDGE('',*,*,#5127,.T.) ;
#7130 = ORIENTED_EDGE('',*,*,#5125,.F.) ;
#7131 = ORIENTED_EDGE('',*,*,#5129,.F.) ;
#7132 = ORIENTED_EDGE('',*,*,#5130,.T.) ;
#7133 = ORIENTED_EDGE('',*,*,#5131,.T.) ;
#7134 = ORIENTED_EDGE('',*,*,#5005,.F.) ;
#7135 = ORIENTED_EDGE('',*,*,#5006,.F.) ;
#7136 = ORIENTED_EDGE('',*,*,#5131,.F.) ;
#7137 = ORIENTED_EDGE('',*,*,#5132,.F.) ;
#7138 = ORIENTED_EDGE('',*,*,#5133,.F.) ;
#7139 = ORIENTED_EDGE('',*,*,#5007,.F.) ;
#7140 = ORIENTED_EDGE('',*,*,#5132,.T.) ;
#7141 = ORIENTED_EDGE('',*,*,#5130,.F.) ;
#7142 = ORIENTED_EDGE('',*,*,#5134,.F.) ;
#7143 = ORIENTED_EDGE('',*,*,#5135,.T.) ;
#7144 = ORIENTED_EDGE('',*,*,#5136,.T.) ;
#7145 = ORIENTED_EDGE('',*,*,#5001,.F.) ;
#7146 = ORIENTED_EDGE('',*,*,#5002,.F.) ;
#7147 = ORIENTED_EDGE('',*,*,#5136,.F.) ;
#7148 = ORIENTED_EDGE('',*,*,#5137,.F.) ;
#7149 = ORIENTED_EDGE('',*,*,#5138,.F.) ;
#7150 = ORIENTED_EDGE('',*,*,#5003,.F.) ;
#7151 = ORIENTED_EDGE('',*,*,#5137,.T.) ;
#7152 = ORIENTED_EDGE('',*,*,#5135,.F.) ;
#7153 = ORIENTED_EDGE('',*,*,#5139,.F.) ;
#7154 = ORIENTED_EDGE('',*,*,#5140,.T.) ;
#7155 = ORIENTED_EDGE('',*,*,#5141,.T.) ;
#7156 = ORIENTED_EDGE('',*,*,#4997,.F.) ;
#7157 = ORIENTED_EDGE('',*,*,#4998,.F.) ;
#7158 = ORIENTED_EDGE('',*,*,#5141,.F.) ;
#7159 = ORIENTED_EDGE('',*,*,#5142,.F.) ;
#7160 = ORIENTED_EDGE('',*,*,#5143,.F.) ;
#7161 = ORIENTED_EDGE('',*,*,#4999,.F.) ;
#7162 = ORIENTED_EDGE('',*,*,#5142,.T.) ;
#7163 = ORIENTED_EDGE('',*,*,#5140,.F.) ;
#7164 = ORIENTED_EDGE('',*,*,#5144,.F.) ;
#7165 = ORIENTED_EDGE('',*,*,#5145,.T.) ;
#7166 = ORIENTED_EDGE('',*,*,#5146,.T.) ;
#7167 = ORIENTED_EDGE('',*,*,#4993,.F.) ;
#7168 = ORIENTED_EDGE('',*,*,#4994,.F.) ;
#7169 = ORIENTED_EDGE('',*,*,#5146,.F.) ;
#7170 = ORIENTED_EDGE('',*,*,#5147,.F.) ;
#7171 = ORIENTED_EDGE('',*,*,#5148,.F.) ;
#7172 = ORIENTED_EDGE('',*,*,#4995,.F.) ;
#7173 = ORIENTED_EDGE('',*,*,#5147,.T.) ;
#7174 = ORIENTED_EDGE('',*,*,#5145,.F.) ;
#7175 = ORIENTED_EDGE('',*,*,#5149,.F.) ;
#7176 = ORIENTED_EDGE('',*,*,#5150,.T.) ;
#7177 = ORIENTED_EDGE('',*,*,#5151,.T.) ;
#7178 = ORIENTED_EDGE('',*,*,#4989,.F.) ;
#7179 = ORIENTED_EDGE('',*,*,#4990,.F.) ;
#7180 = ORIENTED_EDGE('',*,*,#5151,.F.) ;
#7181 = ORIENTED_EDGE('',*,*,#5152,.F.) ;
#7182 = ORIENTED_EDGE('',*,*,#5153,.F.) ;
#7183 = ORIENTED_EDGE('',*,*,#4991,.F.) ;
#7184 = ORIENTED_EDGE('',*,*,#5152,.T.) ;
#7185 = ORIENTED_EDGE('',*,*,#5150,.F.) ;
#7186 = ORIENTED_EDGE('',*,*,#5154,.F.) ;
#7187 = ORIENTED_EDGE('',*,*,#5155,.T.) ;
#7188 = ORIENTED_EDGE('',*,*,#5156,.T.) ;
#7189 = ORIENTED_EDGE('',*,*,#4985,.F.) ;
#7190 = ORIENTED_EDGE('',*,*,#4986,.F.) ;
#7191 = ORIENTED_EDGE('',*,*,#5156,.F.) ;
#7192 = ORIENTED_EDGE('',*,*,#5157,.F.) ;
#7193 = ORIENTED_EDGE('',*,*,#5158,.F.) ;
#7194 = ORIENTED_EDGE('',*,*,#4987,.F.) ;
#7195 = ORIENTED_EDGE('',*,*,#5157,.T.) ;
#7196 = ORIENTED_EDGE('',*,*,#5155,.F.) ;
#7197 = ORIENTED_EDGE('',*,*,#5159,.F.) ;
#7198 = ORIENTED_EDGE('',*,*,#5160,.T.) ;
#7199 = ORIENTED_EDGE('',*,*,#5161,.T.) ;
#7200 = ORIENTED_EDGE('',*,*,#4981,.F.) ;
#7201 = ORIENTED_EDGE('',*,*,#4982,.F.) ;
#7202 = ORIENTED_EDGE('',*,*,#5161,.F.) ;
#7203 = ORIENTED_EDGE('',*,*,#5162,.F.) ;
#7204 = ORIENTED_EDGE('',*,*,#5163,.F.) ;
#7205 = ORIENTED_EDGE('',*,*,#4983,.F.) ;
#7206 = ORIENTED_EDGE('',*,*,#5162,.T.) ;
#7207 = ORIENTED_EDGE('',*,*,#5160,.F.) ;
#7208 = ORIENTED_EDGE('',*,*,#5164,.F.) ;
#7209 = ORIENTED_EDGE('',*,*,#5165,.T.) ;
#7210 = ORIENTED_EDGE('',*,*,#5166,.T.) ;
#7211 = ORIENTED_EDGE('',*,*,#4977,.F.) ;
#7212 = ORIENTED_EDGE('',*,*,#4978,.F.) ;
#7213 = ORIENTED_EDGE('',*,*,#5166,.F.) ;
#7214 = ORIENTED_EDGE('',*,*,#5167,.F.) ;
#7215 = ORIENTED_EDGE('',*,*,#5168,.F.) ;
#7216 = ORIENTED_EDGE('',*,*,#4979,.F.) ;
#7217 = ORIENTED_EDGE('',*,*,#5167,.T.) ;
#7218 = ORIENTED_EDGE('',*,*,#5165,.F.) ;
#7219 = ORIENTED_EDGE('',*,*,#5169,.F.) ;
#7220 = ORIENTED_EDGE('',*,*,#5170,.T.) ;
#7221 = ORIENTED_EDGE('',*,*,#5171,.T.) ;
#7222 = ORIENTED_EDGE('',*,*,#4973,.F.) ;
#7223 = ORIENTED_EDGE('',*,*,#4974,.F.) ;
#7224 = ORIENTED_EDGE('',*,*,#5171,.F.) ;
#7225 = ORIENTED_EDGE('',*,*,#5172,.F.) ;
#7226 = ORIENTED_EDGE('',*,*,#5173,.F.) ;
#7227 = ORIENTED_EDGE('',*,*,#4975,.F.) ;
#7228 = ORIENTED_EDGE('',*,*,#5172,.T.) ;
#7229 = ORIENTED_EDGE('',*,*,#5170,.F.) ;
#7230 = ORIENTED_EDGE('',*,*,#5174,.F.) ;
#7231 = ORIENTED_EDGE('',*,*,#5175,.T.) ;
#7232 = ORIENTED_EDGE('',*,*,#5176,.T.) ;
#7233 = ORIENTED_EDGE('',*,*,#4969,.F.) ;
#7234 = ORIENTED_EDGE('',*,*,#4970,.F.) ;
#7235 = ORIENTED_EDGE('',*,*,#5176,.F.) ;
#7236 = ORIENTED_EDGE('',*,*,#5177,.F.) ;
#7237 = ORIENTED_EDGE('',*,*,#5178,.F.) ;
#7238 = ORIENTED_EDGE('',*,*,#4971,.F.) ;
#7239 = ORIENTED_EDGE('',*,*,#5177,.T.) ;
#7240 = ORIENTED_EDGE('',*,*,#5175,.F.) ;
#7241 = ORIENTED_EDGE('',*,*,#5179,.F.) ;
#7242 = ORIENTED_EDGE('',*,*,#5180,.T.) ;
#7243 = ORIENTED_EDGE('',*,*,#5181,.T.) ;
#7244 = ORIENTED_EDGE('',*,*,#4965,.F.) ;
#7245 = ORIENTED_EDGE('',*,*,#4966,.F.) ;
#7246 = ORIENTED_EDGE('',*,*,#5181,.F.) ;
#7247 = ORIENTED_EDGE('',*,*,#5182,.F.) ;
#7248 = ORIENTED_EDGE('',*,*,#5183,.F.) ;
#7249 = ORIENTED_EDGE('',*,*,#4967,.F.) ;
#7250 = ORIENTED_EDGE('',*,*,#5182,.T.) ;
#7251 = ORIENTED_EDGE('',*,*,#5180,.F.) ;
#7252 = ORIENTED_EDGE('',*,*,#5184,.F.) ;
#7253 = ORIENTED_EDGE('',*,*,#5185,.T.) ;
#7254 = ORIENTED_EDGE('',*,*,#5186,.T.) ;
#7255 = ORIENTED_EDGE('',*,*,#4961,.F.) ;
#7256 = ORIENTED_EDGE('',*,*,#4962,.F.) ;
#7257 = ORIENTED_EDGE('',*,*,#5186,.F.) ;
#7258 = ORIENTED_EDGE('',*,*,#5187,.F.) ;
#7259 = ORIENTED_EDGE('',*,*,#5188,.F.) ;
#7260 = ORIENTED_EDGE('',*,*,#4963,.F.) ;
#7261 = ORIENTED_EDGE('',*,*,#5187,.T.) ;
#7262 = ORIENTED_EDGE('',*,*,#5185,.F.) ;
#7263 = ORIENTED_EDGE('',*,*,#5189,.F.) ;
#7264 = ORIENTED_EDGE('',*,*,#5190,.T.) ;
#7265 = ORIENTED_EDGE('',*,*,#5191,.T.) ;
#7266 = ORIENTED_EDGE('',*,*,#4957,.F.) ;
#7267 = ORIENTED_EDGE('',*,*,#4958,.F.) ;
#7268 = ORIENTED_EDGE('',*,*,#5191,.F.) ;
#7269 = ORIENTED_EDGE('',*,*,#5192,.F.) ;
#7270 = ORIENTED_EDGE('',*,*,#5193,.F.) ;
#7271 = ORIENTED_EDGE('',*,*,#4959,.F.) ;
#7272 = ORIENTED_EDGE('',*,*,#5192,.T.) ;
#7273 = ORIENTED_EDGE('',*,*,#5190,.F.) ;
#7274 = ORIENTED_EDGE('',*,*,#5194,.F.) ;
#7275 = ORIENTED_EDGE('',*,*,#5195,.T.) ;
#7276 = ORIENTED_EDGE('',*,*,#5196,.T.) ;
#7277 = ORIENTED_EDGE('',*,*,#4953,.F.) ;
#7278 = ORIENTED_EDGE('',*,*,#4954,.F.) ;
#7279 = ORIENTED_EDGE('',*,*,#5196,.F.) ;
#7280 = ORIENTED_EDGE('',*,*,#5197,.F.) ;
#7281 = ORIENTED_EDGE('',*,*,#5198,.F.) ;
#7282 = ORIENTED_EDGE('',*,*,#4955,.F.) ;
#7283 = ORIENTED_EDGE('',*,*,#5197,.T.) ;
#7284 = ORIENTED_EDGE('',*,*,#5195,.F.) ;
#7285 = ORIENTED_EDGE('',*,*,#5199,.F.) ;
#7286 = ORIENTED_EDGE('',*,*,#5200,.T.) ;
#7287 = ORIENTED_EDGE('',*,*,#5201,.T.) ;
#7288 = ORIENTED_EDGE('',*,*,#4949,.F.) ;
#7289 = ORIENTED_EDGE('',*,*,#4950,.F.) ;
#7290 = ORIENTED_EDGE('',*,*,#5201,.F.) ;
#7291 = ORIENTED_EDGE('',*,*,#5202,.F.) ;
#7292 = ORIENTED_EDGE('',*,*,#5203,.F.) ;
#7293 = ORIENTED_EDGE('',*,*,#4951,.F.) ;
#7294 = ORIENTED_EDGE('',*,*,#5202,.T.) ;
#7295 = ORIENTED_EDGE('',*,*,#5200,.F.) ;
#7296 = ORIENTED_EDGE('',*,*,#5204,.F.) ;
#7297 = ORIENTED_EDGE('',*,*,#5205,.T.) ;
#7298 = ORIENTED_EDGE('',*,*,#5206,.T.) ;
#7299 = ORIENTED_EDGE('',*,*,#4945,.F.) ;
#7300 = ORIENTED_EDGE('',*,*,#4946,.F.) ;
#7301 = ORIENTED_EDGE('',*,*,#5206,.F.) ;
#7302 = ORIENTED_EDGE('',*,*,#5207,.F.) ;
#7303 = ORIENTED_EDGE('',*,*,#5208,.F.) ;
#7304 = ORIENTED_EDGE('',*,*,#4947,.F.) ;
#7305 = ORIENTED_EDGE('',*,*,#5207,.T.) ;
#7306 = ORIENTED_EDGE('',*,*,#5205,.F.) ;
#7307 = ORIENTED_EDGE('',*,*,#5209,.F.) ;
#7308 = ORIENTED_EDGE('',*,*,#5210,.T.) ;
#7309 = ORIENTED_EDGE('',*,*,#5211,.T.) ;
#7310 = ORIENTED_EDGE('',*,*,#4941,.F.) ;
#7311 = ORIENTED_EDGE('',*,*,#4942,.F.) ;
#7312 = ORIENTED_EDGE('',*,*,#5211,.F.) ;
#7313 = ORIENTED_EDGE('',*,*,#5212,.F.) ;
#7314 = ORIENTED_EDGE('',*,*,#5213,.F.) ;
#7315 = ORIENTED_EDGE('',*,*,#4943,.F.) ;
#7316 = ORIENTED_EDGE('',*,*,#5212,.T.) ;
#7317 = ORIENTED_EDGE('',*,*,#5210,.F.) ;
#7318 = ORIENTED_EDGE('',*,*,#5214,.F.) ;
#7319 = ORIENTED_EDGE('',*,*,#5215,.T.) ;
#7320 = ORIENTED_EDGE('',*,*,#5216,.T.) ;
#7321 = ORIENTED_EDGE('',*,*,#4937,.F.) ;
#7322 = ORIENTED_EDGE('',*,*,#4938,.F.) ;
#7323 = ORIENTED_EDGE('',*,*,#5216,.F.) ;
#7324 = ORIENTED_EDGE('',*,*,#5217,.F.) ;
#7325 = ORIENTED_EDGE('',*,*,#5218,.F.) ;
#7326 = ORIENTED_EDGE('',*,*,#4939,.F.) ;
#7327 = ORIENTED_EDGE('',*,*,#5217,.T.) ;
#7328 = ORIENTED_EDGE('',*,*,#5215,.F.) ;
#7329 = ORIENTED_EDGE('',*,*,#5219,.F.) ;
#7330 = ORIENTED_EDGE('',*,*,#5220,.T.) ;
#7331 = ORIENTED_EDGE('',*,*,#5221,.T.) ;
#7332 = ORIENTED_EDGE('',*,*,#4933,.F.) ;
#7333 = ORIENTED_EDGE('',*,*,#4934,.F.) ;
#7334 = ORIENTED_EDGE('',*,*,#5221,.F.) ;
#7335 = ORIENTED_EDGE('',*,*,#5222,.F.) ;
#7336 = ORIENTED_EDGE('',*,*,#5223,.F.) ;
#7337 = ORIENTED_EDGE('',*,*,#4935,.F.) ;
#7338 = ORIENTED_EDGE('',*,*,#5222,.T.) ;
#7339 = ORIENTED_EDGE('',*,*,#5220,.F.) ;
#7340 = ORIENTED_EDGE('',*,*,#5224,.F.) ;
#7341 = ORIENTED_EDGE('',*,*,#5225,.T.) ;
#7342 = ORIENTED_EDGE('',*,*,#5226,.T.) ;
#7343 = ORIENTED_EDGE('',*,*,#4929,.F.) ;
#7344 = ORIENTED_EDGE('',*,*,#4930,.F.) ;
#7345 = ORIENTED_EDGE('',*,*,#5226,.F.) ;
#7346 = ORIENTED_EDGE('',*,*,#5227,.F.) ;
#7347 = ORIENTED_EDGE('',*,*,#5228,.F.) ;
#7348 = ORIENTED_EDGE('',*,*,#4931,.F.) ;
#7349 = ORIENTED_EDGE('',*,*,#5227,.T.) ;
#7350 = ORIENTED_EDGE('',*,*,#5225,.F.) ;
#7351 = ORIENTED_EDGE('',*,*,#5229,.F.) ;
#7352 = ORIENTED_EDGE('',*,*,#5230,.T.) ;
#7353 = ORIENTED_EDGE('',*,*,#5231,.T.) ;
#7354 = ORIENTED_EDGE('',*,*,#4925,.F.) ;
#7355 = ORIENTED_EDGE('',*,*,#4926,.F.) ;
#7356 = ORIENTED_EDGE('',*,*,#5231,.F.) ;
#7357 = ORIENTED_EDGE('',*,*,#5232,.F.) ;
#7358 = ORIENTED_EDGE('',*,*,#5233,.F.) ;
#7359 = ORIENTED_EDGE('',*,*,#4927,.F.) ;
#7360 = ORIENTED_EDGE('',*,*,#5232,.T.) ;
#7361 = ORIENTED_EDGE('',*,*,#5230,.F.) ;
#7362 = ORIENTED_EDGE('',*,*,#5234,.F.) ;
#7363 = ORIENTED_EDGE('',*,*,#5235,.T.) ;
#7364 = ORIENTED_EDGE('',*,*,#5236,.T.) ;
#7365 = ORIENTED_EDGE('',*,*,#4921,.F.) ;
#7366 = ORIENTED_EDGE('',*,*,#4922,.F.) ;
#7367 = ORIENTED_EDGE('',*,*,#5236,.F.) ;
#7368 = ORIENTED_EDGE('',*,*,#5237,.F.) ;
#7369 = ORIENTED_EDGE('',*,*,#5238,.F.) ;
#7370 = ORIENTED_EDGE('',*,*,#4923,.F.) ;
#7371 = ORIENTED_EDGE('',*,*,#5237,.T.) ;
#7372 = ORIENTED_EDGE('',*,*,#5235,.F.) ;
#7373 = ORIENTED_EDGE('',*,*,#5032,.T.) ;
#7374 = ORIENTED_EDGE('',*,*,#5239,.T.) ;
#7375 = ORIENTED_EDGE('',*,*,#4909,.T.) ;
#7376 = ORIENTED_EDGE('',*,*,#5239,.F.) ;
#7377 = ORIENTED_EDGE('',*,*,#5240,.T.) ;
#7378 = ORIENTED_EDGE('',*,*,#5241,.T.) ;
#7379 = ORIENTED_EDGE('',*,*,#5099,.T.) ;
#7380 = ORIENTED_EDGE('',*,*,#5028,.T.) ;
#7381 = ORIENTED_EDGE('',*,*,#5108,.T.) ;
#7382 = ORIENTED_EDGE('',*,*,#5104,.T.) ;
#7383 = ORIENTED_EDGE('',*,*,#5024,.T.) ;
#7384 = ORIENTED_EDGE('',*,*,#5113,.T.) ;
#7385 = ORIENTED_EDGE('',*,*,#5109,.T.) ;
#7386 = ORIENTED_EDGE('',*,*,#5020,.T.) ;
#7387 = ORIENTED_EDGE('',*,*,#5118,.T.) ;
#7388 = ORIENTED_EDGE('',*,*,#5114,.T.) ;
#7389 = ORIENTED_EDGE('',*,*,#5016,.T.) ;
#7390 = ORIENTED_EDGE('',*,*,#5123,.T.) ;
#7391 = ORIENTED_EDGE('',*,*,#5119,.T.) ;
#7392 = ORIENTED_EDGE('',*,*,#5012,.T.) ;
#7393 = ORIENTED_EDGE('',*,*,#5128,.T.) ;
#7394 = ORIENTED_EDGE('',*,*,#5124,.T.) ;
#7395 = ORIENTED_EDGE('',*,*,#5008,.T.) ;
#7396 = ORIENTED_EDGE('',*,*,#5133,.T.) ;
#7397 = ORIENTED_EDGE('',*,*,#5129,.T.) ;
#7398 = ORIENTED_EDGE('',*,*,#5004,.T.) ;
#7399 = ORIENTED_EDGE('',*,*,#5138,.T.) ;
#7400 = ORIENTED_EDGE('',*,*,#5134,.T.) ;
#7401 = ORIENTED_EDGE('',*,*,#5000,.T.) ;
#7402 = ORIENTED_EDGE('',*,*,#5143,.T.) ;
#7403 = ORIENTED_EDGE('',*,*,#5139,.T.) ;
#7404 = ORIENTED_EDGE('',*,*,#4996,.T.) ;
#7405 = ORIENTED_EDGE('',*,*,#5148,.T.) ;
#7406 = ORIENTED_EDGE('',*,*,#5144,.T.) ;
#7407 = ORIENTED_EDGE('',*,*,#4992,.T.) ;
#7408 = ORIENTED_EDGE('',*,*,#5153,.T.) ;
#7409 = ORIENTED_EDGE('',*,*,#5149,.T.) ;
#7410 = ORIENTED_EDGE('',*,*,#4988,.T.) ;
#7411 = ORIENTED_EDGE('',*,*,#5158,.T.) ;
#7412 = ORIENTED_EDGE('',*,*,#5154,.T.) ;
#7413 = ORIENTED_EDGE('',*,*,#4984,.T.) ;
#7414 = ORIENTED_EDGE('',*,*,#5163,.T.) ;
#7415 = ORIENTED_EDGE('',*,*,#5159,.T.) ;
#7416 = ORIENTED_EDGE('',*,*,#4980,.T.) ;
#7417 = ORIENTED_EDGE('',*,*,#5168,.T.) ;
#7418 = ORIENTED_EDGE('',*,*,#5164,.T.) ;
#7419 = ORIENTED_EDGE('',*,*,#4976,.T.) ;
#7420 = ORIENTED_EDGE('',*,*,#5173,.T.) ;
#7421 = ORIENTED_EDGE('',*,*,#5169,.T.) ;
#7422 = ORIENTED_EDGE('',*,*,#4972,.T.) ;
#7423 = ORIENTED_EDGE('',*,*,#5178,.T.) ;
#7424 = ORIENTED_EDGE('',*,*,#5174,.T.) ;
#7425 = ORIENTED_EDGE('',*,*,#4968,.T.) ;
#7426 = ORIENTED_EDGE('',*,*,#5183,.T.) ;
#7427 = ORIENTED_EDGE('',*,*,#5179,.T.) ;
#7428 = ORIENTED_EDGE('',*,*,#4964,.T.) ;
#7429 = ORIENTED_EDGE('',*,*,#5188,.T.) ;
#7430 = ORIENTED_EDGE('',*,*,#5184,.T.) ;
#7431 = ORIENTED_EDGE('',*,*,#4960,.T.) ;
#7432 = ORIENTED_EDGE('',*,*,#5193,.T.) ;
#7433 = ORIENTED_EDGE('',*,*,#5189,.T.) ;
#7434 = ORIENTED_EDGE('',*,*,#4956,.T.) ;
#7435 = ORIENTED_EDGE('',*,*,#5198,.T.) ;
#7436 = ORIENTED_EDGE('',*,*,#5194,.T.) ;
#7437 = ORIENTED_EDGE('',*,*,#4952,.T.) ;
#7438 = ORIENTED_EDGE('',*,*,#5203,.T.) ;
#7439 = ORIENTED_EDGE('',*,*,#5199,.T.) ;
#7440 = ORIENTED_EDGE('',*,*,#4948,.T.) ;
#7441 = ORIENTED_EDGE('',*,*,#5208,.T.) ;
#7442 = ORIENTED_EDGE('',*,*,#5204,.T.) ;
#7443 = ORIENTED_EDGE('',*,*,#4944,.T.) ;
#7444 = ORIENTED_EDGE('',*,*,#5213,.T.) ;
#7445 = ORIENTED_EDGE('',*,*,#5209,.T.) ;
#7446 = ORIENTED_EDGE('',*,*,#4940,.T.) ;
#7447 = ORIENTED_EDGE('',*,*,#5218,.T.) ;
#7448 = ORIENTED_EDGE('',*,*,#5214,.T.) ;
#7449 = ORIENTED_EDGE('',*,*,#4936,.T.) ;
#7450 = ORIENTED_EDGE('',*,*,#5223,.T.) ;
#7451 = ORIENTED_EDGE('',*,*,#5219,.T.) ;
#7452 = ORIENTED_EDGE('',*,*,#4932,.T.) ;
#7453 = ORIENTED_EDGE('',*,*,#5228,.T.) ;
#7454 = ORIENTED_EDGE('',*,*,#5224,.T.) ;
#7455 = ORIENTED_EDGE('',*,*,#4928,.T.) ;
#7456 = ORIENTED_EDGE('',*,*,#5233,.T.) ;
#7457 = ORIENTED_EDGE('',*,*,#5229,.T.) ;
#7458 = ORIENTED_EDGE('',*,*,#4924,.T.) ;
#7459 = ORIENTED_EDGE('',*,*,#5238,.T.) ;
#7460 = ORIENTED_EDGE('',*,*,#5234,.T.) ;
#7461 = ORIENTED_EDGE('',*,*,#4920,.T.) ;
#7462 = ORIENTED_EDGE('',*,*,#4918,.T.) ;
#7463 = ORIENTED_EDGE('',*,*,#4912,.T.) ;
#7464 = ORIENTED_EDGE('',*,*,#5063,.T.) ;
#7465 = ORIENTED_EDGE('',*,*,#5068,.T.) ;
#7466 = ORIENTED_EDGE('',*,*,#5064,.T.) ;
#7467 = ORIENTED_EDGE('',*,*,#5059,.T.) ;
#7468 = ORIENTED_EDGE('',*,*,#5073,.T.) ;
#7469 = ORIENTED_EDGE('',*,*,#5069,.T.) ;
#7470 = ORIENTED_EDGE('',*,*,#5055,.T.) ;
#7471 = ORIENTED_EDGE('',*,*,#5078,.T.) ;
#7472 = ORIENTED_EDGE('',*,*,#5074,.T.) ;
#7473 = ORIENTED_EDGE('',*,*,#5051,.T.) ;
#7474 = ORIENTED_EDGE('',*,*,#5083,.T.) ;
#7475 = ORIENTED_EDGE('',*,*,#5079,.T.) ;
#7476 = ORIENTED_EDGE('',*,*,#5047,.T.) ;
#7477 = ORIENTED_EDGE('',*,*,#5088,.T.) ;
#7478 = ORIENTED_EDGE('',*,*,#5084,.T.) ;
#7479 = ORIENTED_EDGE('',*,*,#5043,.T.) ;
#7480 = ORIENTED_EDGE('',*,*,#5093,.T.) ;
#7481 = ORIENTED_EDGE('',*,*,#5089,.T.) ;
#7482 = ORIENTED_EDGE('',*,*,#5039,.T.) ;
#7483 = ORIENTED_EDGE('',*,*,#5098,.T.) ;
#7484 = ORIENTED_EDGE('',*,*,#5094,.T.) ;
#7485 = ORIENTED_EDGE('',*,*,#5035,.T.) ;
#7486 = ORIENTED_EDGE('',*,*,#5103,.T.) ;
#7487 = ORIENTED_EDGE('',*,*,#5241,.F.) ;
#7488 = ORIENTED_EDGE('',*,*,#5240,.F.) ;
#7489 = ORIENTED_EDGE('',*,*,#5242,.T.) ;
#7490 = ORIENTED_EDGE('',*,*,#5243,.F.) ;
#7491 = ORIENTED_EDGE('',*,*,#5244,.F.) ;
#7492 = ORIENTED_EDGE('',*,*,#5245,.F.) ;
#7493 = ORIENTED_EDGE('',*,*,#5246,.F.) ;
#7494 = ORIENTED_EDGE('',*,*,#5247,.F.) ;
#7495 = ORIENTED_EDGE('',*,*,#5248,.F.) ;
#7496 = ORIENTED_EDGE('',*,*,#5249,.F.) ;
#7497 = ORIENTED_EDGE('',*,*,#5250,.F.) ;
#7498 = ORIENTED_EDGE('',*,*,#5251,.F.) ;
#7499 = ORIENTED_EDGE('',*,*,#5252,.F.) ;
#7500 = ORIENTED_EDGE('',*,*,#5253,.F.) ;
#7501 = ORIENTED_EDGE('',*,*,#5254,.F.) ;
#7502 = ORIENTED_EDGE('',*,*,#5255,.F.) ;
#7503 = ORIENTED_EDGE('',*,*,#5256,.F.) ;
#7504 = ORIENTED_EDGE('',*,*,#5257,.F.) ;
#7505 = ORIENTED_EDGE('',*,*,#5258,.T.) ;
#7506 = ORIENTED_EDGE('',*,*,#5242,.F.) ;
#7507 = ORIENTED_EDGE('',*,*,#5258,.F.) ;
#7508 = ORIENTED_EDGE('',*,*,#5259,.F.) ;
#7509 = ORIENTED_EDGE('',*,*,#5260,.F.) ;
#7510 = ORIENTED_EDGE('',*,*,#5261,.F.) ;
#7511 = ORIENTED_EDGE('',*,*,#5262,.F.) ;
#7512 = ORIENTED_EDGE('',*,*,#5253,.T.) ;
#7513 = ORIENTED_EDGE('',*,*,#5263,.F.) ;
#7514 = ORIENTED_EDGE('',*,*,#5264,.F.) ;
#7515 = ORIENTED_EDGE('',*,*,#5265,.F.) ;
#7516 = ORIENTED_EDGE('',*,*,#5266,.F.) ;
#7517 = ORIENTED_EDGE('',*,*,#5267,.F.) ;
#7518 = ORIENTED_EDGE('',*,*,#5250,.T.) ;
#7519 = ORIENTED_EDGE('',*,*,#5268,.F.) ;
#7520 = ORIENTED_EDGE('',*,*,#5256,.T.) ;
#7521 = ORIENTED_EDGE('',*,*,#5269,.F.) ;
#7522 = ORIENTED_EDGE('',*,*,#5270,.F.) ;
#7523 = ORIENTED_EDGE('',*,*,#5271,.F.) ;
#7524 = ORIENTED_EDGE('',*,*,#5272,.F.) ;
#7525 = ORIENTED_EDGE('',*,*,#5273,.F.) ;
#7526 = ORIENTED_EDGE('',*,*,#5247,.T.) ;
#7527 = ORIENTED_EDGE('',*,*,#5274,.F.) ;
#7528 = ORIENTED_EDGE('',*,*,#5260,.T.) ;
#7529 = ORIENTED_EDGE('',*,*,#5275,.F.) ;
#7530 = ORIENTED_EDGE('',*,*,#5276,.F.) ;
#7531 = ORIENTED_EDGE('',*,*,#5277,.F.) ;
#7532 = ORIENTED_EDGE('',*,*,#5278,.F.) ;
#7533 = ORIENTED_EDGE('',*,*,#5279,.F.) ;
#7534 = ORIENTED_EDGE('',*,*,#5244,.T.) ;
#7535 = ORIENTED_EDGE('',*,*,#5261,.T.) ;
#7536 = ORIENTED_EDGE('',*,*,#5274,.T.) ;
#7537 = ORIENTED_EDGE('',*,*,#5280,.F.) ;
#7538 = ORIENTED_EDGE('',*,*,#5275,.T.) ;
#7539 = ORIENTED_EDGE('',*,*,#5259,.T.) ;
#7540 = ORIENTED_EDGE('',*,*,#5281,.T.) ;
#7541 = ORIENTED_EDGE('',*,*,#5282,.T.) ;
#7542 = ORIENTED_EDGE('',*,*,#5283,.F.) ;
#7543 = ORIENTED_EDGE('',*,*,#5257,.T.) ;
#7544 = ORIENTED_EDGE('',*,*,#5268,.T.) ;
#7545 = ORIENTED_EDGE('',*,*,#5284,.F.) ;
#7546 = ORIENTED_EDGE('',*,*,#5269,.T.) ;
#7547 = ORIENTED_EDGE('',*,*,#5255,.T.) ;
#7548 = ORIENTED_EDGE('',*,*,#5285,.T.) ;
#7549 = ORIENTED_EDGE('',*,*,#5286,.T.) ;
#7550 = ORIENTED_EDGE('',*,*,#5281,.F.) ;
#7551 = ORIENTED_EDGE('',*,*,#5254,.T.) ;
#7552 = ORIENTED_EDGE('',*,*,#5262,.T.) ;
#7553 = ORIENTED_EDGE('',*,*,#5287,.F.) ;
#7554 = ORIENTED_EDGE('',*,*,#5263,.T.) ;
#7555 = ORIENTED_EDGE('',*,*,#5252,.T.) ;
#7556 = ORIENTED_EDGE('',*,*,#5288,.T.) ;
#7557 = ORIENTED_EDGE('',*,*,#5289,.T.) ;
#7558 = ORIENTED_EDGE('',*,*,#5285,.F.) ;
#7559 = ORIENTED_EDGE('',*,*,#5264,.T.) ;
#7560 = ORIENTED_EDGE('',*,*,#5287,.T.) ;
#7561 = ORIENTED_EDGE('',*,*,#5270,.T.) ;
#7562 = ORIENTED_EDGE('',*,*,#5284,.T.) ;
#7563 = ORIENTED_EDGE('',*,*,#5266,.T.) ;
#7564 = ORIENTED_EDGE('',*,*,#5290,.T.) ;
#7565 = ORIENTED_EDGE('',*,*,#5276,.T.) ;
#7566 = ORIENTED_EDGE('',*,*,#5280,.T.) ;
#7567 = ORIENTED_EDGE('',*,*,#5272,.T.) ;
#7568 = ORIENTED_EDGE('',*,*,#5291,.T.) ;
#7569 = ORIENTED_EDGE('',*,*,#5278,.T.) ;
#7570 = ORIENTED_EDGE('',*,*,#5292,.T.) ;
#7571 = ORIENTED_EDGE('',*,*,#5293,.F.) ;
#7572 = ORIENTED_EDGE('',*,*,#5294,.F.) ;
#7573 = ORIENTED_EDGE('',*,*,#5295,.F.) ;
#7574 = ORIENTED_EDGE('',*,*,#5296,.F.) ;
#7575 = ORIENTED_EDGE('',*,*,#5289,.F.) ;
#7576 = ORIENTED_EDGE('',*,*,#5297,.F.) ;
#7577 = ORIENTED_EDGE('',*,*,#5286,.F.) ;
#7578 = ORIENTED_EDGE('',*,*,#5298,.F.) ;
#7579 = ORIENTED_EDGE('',*,*,#5282,.F.) ;
#7580 = ORIENTED_EDGE('',*,*,#5299,.F.) ;
#7581 = ORIENTED_EDGE('',*,*,#5300,.F.) ;
#7582 = ORIENTED_EDGE('',*,*,#5301,.F.) ;
#7583 = ORIENTED_EDGE('',*,*,#5302,.T.) ;
#7584 = ORIENTED_EDGE('',*,*,#5298,.T.) ;
#7585 = ORIENTED_EDGE('',*,*,#5297,.T.) ;
#7586 = ORIENTED_EDGE('',*,*,#5296,.T.) ;
#7587 = ORIENTED_EDGE('',*,*,#5294,.T.) ;
#7588 = ORIENTED_EDGE('',*,*,#5301,.T.) ;
#7589 = ORIENTED_EDGE('',*,*,#5299,.T.) ;
#7590 = ORIENTED_EDGE('',*,*,#5302,.F.) ;
#7591 = ORIENTED_EDGE('',*,*,#5246,.T.) ;
#7592 = ORIENTED_EDGE('',*,*,#5303,.T.) ;
#7593 = ORIENTED_EDGE('',*,*,#5293,.T.) ;
#7594 = ORIENTED_EDGE('',*,*,#5304,.F.) ;
#7595 = ORIENTED_EDGE('',*,*,#5248,.T.) ;
#7596 = ORIENTED_EDGE('',*,*,#5273,.T.) ;
#7597 = ORIENTED_EDGE('',*,*,#5291,.F.) ;
#7598 = ORIENTED_EDGE('',*,*,#5271,.T.) ;
#7599 = ORIENTED_EDGE('',*,*,#5243,.T.) ;
#7600 = ORIENTED_EDGE('',*,*,#5283,.T.) ;
#7601 = ORIENTED_EDGE('',*,*,#5300,.T.) ;
#7602 = ORIENTED_EDGE('',*,*,#5303,.F.) ;
#7603 = ORIENTED_EDGE('',*,*,#5245,.T.) ;
#7604 = ORIENTED_EDGE('',*,*,#5279,.T.) ;
#7605 = ORIENTED_EDGE('',*,*,#5292,.F.) ;
#7606 = ORIENTED_EDGE('',*,*,#5277,.T.) ;
#7607 = ORIENTED_EDGE('',*,*,#5249,.T.) ;
#7608 = ORIENTED_EDGE('',*,*,#5304,.T.) ;
#7609 = ORIENTED_EDGE('',*,*,#5295,.T.) ;
#7610 = ORIENTED_EDGE('',*,*,#5288,.F.) ;
#7611 = ORIENTED_EDGE('',*,*,#5251,.T.) ;
#7612 = ORIENTED_EDGE('',*,*,#5267,.T.) ;
#7613 = ORIENTED_EDGE('',*,*,#5290,.F.) ;
#7614 = ORIENTED_EDGE('',*,*,#5265,.T.) ;
#7615 = ORIENTED_EDGE('',*,*,#5305,.F.) ;
#7616 = ORIENTED_EDGE('',*,*,#5306,.T.) ;
#7617 = ORIENTED_EDGE('',*,*,#5307,.F.) ;
#7618 = ORIENTED_EDGE('',*,*,#5308,.T.) ;
#7619 = ORIENTED_EDGE('',*,*,#5305,.T.) ;
#7620 = ORIENTED_EDGE('',*,*,#5308,.F.) ;
#7621 = ORIENTED_EDGE('',*,*,#5307,.T.) ;
#7622 = ORIENTED_EDGE('',*,*,#5309,.F.) ;
#7623 = ORIENTED_EDGE('',*,*,#5309,.T.) ;
#7624 = ORIENTED_EDGE('',*,*,#5310,.T.) ;
#7625 = ORIENTED_EDGE('',*,*,#5311,.F.) ;
#7626 = ORIENTED_EDGE('',*,*,#5310,.F.) ;
#7627 = ORIENTED_EDGE('',*,*,#5311,.T.) ;
#7628 = ORIENTED_EDGE('',*,*,#5312,.T.) ;
#7629 = ORIENTED_EDGE('',*,*,#5313,.F.) ;
#7630 = ORIENTED_EDGE('',*,*,#5312,.F.) ;
#7631 = ORIENTED_EDGE('',*,*,#5313,.T.) ;
#7632 = ORIENTED_EDGE('',*,*,#5314,.T.) ;
#7633 = ORIENTED_EDGE('',*,*,#5315,.F.) ;
#7634 = ORIENTED_EDGE('',*,*,#5314,.F.) ;
#7635 = ORIENTED_EDGE('',*,*,#5315,.T.) ;
#7636 = ORIENTED_EDGE('',*,*,#5316,.T.) ;
#7637 = ORIENTED_EDGE('',*,*,#5317,.F.) ;
#7638 = ORIENTED_EDGE('',*,*,#5316,.F.) ;
#7639 = ORIENTED_EDGE('',*,*,#5317,.T.) ;
#7640 = ORIENTED_EDGE('',*,*,#5318,.T.) ;
#7641 = ORIENTED_EDGE('',*,*,#5319,.F.) ;
#7642 = ORIENTED_EDGE('',*,*,#5318,.F.) ;
#7643 = ORIENTED_EDGE('',*,*,#5319,.T.) ;
#7644 = ORIENTED_EDGE('',*,*,#5320,.T.) ;
#7645 = ORIENTED_EDGE('',*,*,#5306,.F.) ;
#7646 = ORIENTED_EDGE('',*,*,#5320,.F.) ;
#7647 = ORIENTED_EDGE('',*,*,#5321,.F.) ;
#7648 = ORIENTED_EDGE('',*,*,#5322,.T.) ;
#7649 = ORIENTED_EDGE('',*,*,#5323,.F.) ;
#7650 = ORIENTED_EDGE('',*,*,#5322,.F.) ;
#7651 = ORIENTED_EDGE('',*,*,#5324,.F.) ;
#7652 = ORIENTED_EDGE('',*,*,#5325,.F.) ;
#7653 = ORIENTED_EDGE('',*,*,#5326,.F.) ;
#7654 = ORIENTED_EDGE('',*,*,#5327,.F.) ;
#7655 = ORIENTED_EDGE('',*,*,#5328,.F.) ;
#7656 = ORIENTED_EDGE('',*,*,#5326,.T.) ;
#7657 = ORIENTED_EDGE('',*,*,#5329,.F.) ;
#7658 = ORIENTED_EDGE('',*,*,#5330,.F.) ;
#7659 = ORIENTED_EDGE('',*,*,#5331,.F.) ;
#7660 = ORIENTED_EDGE('',*,*,#5332,.F.) ;
#7661 = ORIENTED_EDGE('',*,*,#5333,.F.) ;
#7662 = ORIENTED_EDGE('',*,*,#5330,.T.) ;
#7663 = ORIENTED_EDGE('',*,*,#5331,.T.) ;
#7664 = ORIENTED_EDGE('',*,*,#5329,.T.) ;
#7665 = ORIENTED_EDGE('',*,*,#5325,.T.) ;
#7666 = ORIENTED_EDGE('',*,*,#5334,.T.) ;
#7667 = ORIENTED_EDGE('',*,*,#5335,.T.) ;
#7668 = ORIENTED_EDGE('',*,*,#5336,.T.) ;
#7669 = ORIENTED_EDGE('',*,*,#5337,.T.) ;
#7670 = ORIENTED_EDGE('',*,*,#5338,.T.) ;
#7671 = ORIENTED_EDGE('',*,*,#5323,.T.) ;
#7672 = ORIENTED_EDGE('',*,*,#5339,.T.) ;
#7673 = ORIENTED_EDGE('',*,*,#5340,.F.) ;
#7674 = ORIENTED_EDGE('',*,*,#5341,.T.) ;
#7675 = ORIENTED_EDGE('',*,*,#5339,.F.) ;
#7676 = ORIENTED_EDGE('',*,*,#5341,.F.) ;
#7677 = ORIENTED_EDGE('',*,*,#5342,.F.) ;
#7678 = ORIENTED_EDGE('',*,*,#5343,.T.) ;
#7679 = ORIENTED_EDGE('',*,*,#5344,.T.) ;
#7680 = ORIENTED_EDGE('',*,*,#5335,.F.) ;
#7681 = ORIENTED_EDGE('',*,*,#5345,.T.) ;
#7682 = ORIENTED_EDGE('',*,*,#5346,.T.) ;
#7683 = ORIENTED_EDGE('',*,*,#5336,.F.) ;
#7684 = ORIENTED_EDGE('',*,*,#5344,.F.) ;
#7685 = ORIENTED_EDGE('',*,*,#5324,.T.) ;
#7686 = ORIENTED_EDGE('',*,*,#5347,.T.) ;
#7687 = ORIENTED_EDGE('',*,*,#5342,.T.) ;
#7688 = ORIENTED_EDGE('',*,*,#5334,.F.) ;
#7689 = ORIENTED_EDGE('',*,*,#5348,.F.) ;
#7690 = ORIENTED_EDGE('',*,*,#5349,.F.) ;
#7691 = ORIENTED_EDGE('',*,*,#5337,.F.) ;
#7692 = ORIENTED_EDGE('',*,*,#5346,.F.) ;
#7693 = ORIENTED_EDGE('',*,*,#5349,.T.) ;
#7694 = ORIENTED_EDGE('',*,*,#5350,.T.) ;
#7695 = ORIENTED_EDGE('',*,*,#5332,.T.) ;
#7696 = ORIENTED_EDGE('',*,*,#5338,.F.) ;
#7697 = ORIENTED_EDGE('',*,*,#5333,.T.) ;
#7698 = ORIENTED_EDGE('',*,*,#5350,.F.) ;
#7699 = ORIENTED_EDGE('',*,*,#5348,.T.) ;
#7700 = ORIENTED_EDGE('',*,*,#5345,.F.) ;
#7701 = ORIENTED_EDGE('',*,*,#5343,.F.) ;
#7702 = ORIENTED_EDGE('',*,*,#5347,.F.) ;
#7703 = ORIENTED_EDGE('',*,*,#5327,.T.) ;
#7704 = ORIENTED_EDGE('',*,*,#5328,.T.) ;
#7705 = ORIENTED_EDGE('',*,*,#5321,.T.) ;
#7706 = ORIENTED_EDGE('',*,*,#5340,.T.) ;
#7707 = CONICAL_SURFACE('',#8265,4.3,0.785398163397439) ;
#7708 = CONICAL_SURFACE('',#8273,2.025,1.02974425867665) ;
#7709 = CONICAL_SURFACE('',#8274,4.3,0.785398163397447) ;
#7710 = CONICAL_SURFACE('',#8282,4.05,1.02974425867666) ;
#7711 = CONICAL_SURFACE('',#8307,7.85,0.785398163397456) ;
#7712 = CONICAL_SURFACE('',#8310,7.85,0.785398163397456) ;
#7713 = CONICAL_SURFACE('',#8313,7.85,0.785398163397456) ;
#7714 = CONICAL_SURFACE('',#8316,7.85,0.785398163397456) ;
#7715 = CONICAL_SURFACE('',#8327,7.85,0.785398163397445) ;
#7716 = CONICAL_SURFACE('',#8329,7.85,0.785398163397445) ;
#7717 = CONICAL_SURFACE('',#8331,7.85,0.785398163397445) ;
#7718 = CONICAL_SURFACE('',#8333,7.85,0.785398163397445) ;
#7719 = CONICAL_SURFACE('',#8337,5.75,0.785398163397447) ;
#7720 = CONICAL_SURFACE('',#8344,5.75,0.785398163397439) ;
#7721 = CONICAL_SURFACE('',#8442,4.15,0.785398163397448) ;
#7722 = CONICAL_SURFACE('',#8457,4.15,0.785398163397448) ;
#7723 = CONICAL_SURFACE('',#8463,4.15,0.785398163397452) ;
#7724 = CONICAL_SURFACE('',#8469,4.15,0.785398163397452) ;
#7725 = CONICAL_SURFACE('',#8543,25.25,0.785398163397448) ;
#7726 = CONICAL_SURFACE('',#8547,25.25,0.785398163397448) ;
#7727 = CONICAL_SURFACE('',#8548,15.25,0.785398163397448) ;
#7728 = CONICAL_SURFACE('',#8641,1.704,0.785398163397448) ;
#7729 = CONICAL_SURFACE('',#8829,3.3,0.785398163397448) ;
#7730 = CONICAL_SURFACE('',#8833,1.83205080756888,0.785398163397456) ;
#7731 = CONICAL_SURFACE('',#8873,0.866025403784438,1.02974425867665) ;
#7732 = CONICAL_SURFACE('',#8885,8.625,0.906750163968216) ;
#7733 = CONICAL_SURFACE('',#8889,8.325,1.00406710927139) ;
#7734 = CONICAL_SURFACE('',#8891,8.325,1.00406710927139) ;
#7735 = CONICAL_SURFACE('',#8895,8.525,1.08631839775788) ;
#7736 = ADVANCED_FACE('',(#1061),#7707,.F.) ;
#7737 = ADVANCED_FACE('',(#1062),#977,.F.) ;
#7738 = ADVANCED_FACE('',(#1063,#686),#737,.T.) ;
#7739 = ADVANCED_FACE('',(#1064),#7708,.F.) ;
#7740 = ADVANCED_FACE('',(#1065),#7709,.F.) ;
#7741 = ADVANCED_FACE('',(#1066),#978,.F.) ;
#7742 = ADVANCED_FACE('',(#1067,#687),#738,.T.) ;
#7743 = ADVANCED_FACE('',(#1068),#7710,.F.) ;
#7744 = ADVANCED_FACE('',(#1069),#739,.F.) ;
#7745 = ADVANCED_FACE('',(#1070),#740,.F.) ;
#7746 = ADVANCED_FACE('',(#1071),#741,.T.) ;
#7747 = ADVANCED_FACE('',(#1072),#742,.T.) ;
#7748 = ADVANCED_FACE('',(#1073),#743,.F.) ;
#7749 = ADVANCED_FACE('',(#1074),#744,.F.) ;
#7750 = ADVANCED_FACE('',(#1075),#979,.F.) ;
#7751 = ADVANCED_FACE('',(#1076),#980,.F.) ;
#7752 = ADVANCED_FACE('',(#1077),#981,.F.) ;
#7753 = ADVANCED_FACE('',(#1078),#982,.F.) ;
#7754 = ADVANCED_FACE('',(#1079),#7711,.T.) ;
#7755 = ADVANCED_FACE('',(#1080),#7712,.T.) ;
#7756 = ADVANCED_FACE('',(#1081),#7713,.T.) ;
#7757 = ADVANCED_FACE('',(#1082),#7714,.T.) ;
#7758 = ADVANCED_FACE('',(#1083),#983,.T.) ;
#7759 = ADVANCED_FACE('',(#1084),#984,.T.) ;
#7760 = ADVANCED_FACE('',(#1085),#985,.T.) ;
#7761 = ADVANCED_FACE('',(#1086),#986,.T.) ;
#7762 = ADVANCED_FACE('',(#1087),#7715,.T.) ;
#7763 = ADVANCED_FACE('',(#1088),#7716,.T.) ;
#7764 = ADVANCED_FACE('',(#1089),#7717,.T.) ;
#7765 = ADVANCED_FACE('',(#1090),#7718,.T.) ;
#7766 = ADVANCED_FACE('',(#1091,#688),#745,.T.) ;
#7767 = ADVANCED_FACE('',(#1092),#7719,.T.) ;
#7768 = ADVANCED_FACE('',(#1093),#987,.T.) ;
#7769 = ADVANCED_FACE('',(#1094,#689),#746,.T.) ;
#7770 = ADVANCED_FACE('',(#1095,#690),#988,.T.) ;
#7771 = ADVANCED_FACE('',(#1096),#7720,.T.) ;
#7772 = ADVANCED_FACE('',(#1097),#330,.F.) ;
#7773 = ADVANCED_FACE('',(#1098),#331,.F.) ;
#7774 = ADVANCED_FACE('',(#1099),#332,.F.) ;
#7775 = ADVANCED_FACE('',(#1100),#333,.F.) ;
#7776 = ADVANCED_FACE('',(#1101),#334,.F.) ;
#7777 = ADVANCED_FACE('',(#1102),#335,.F.) ;
#7778 = ADVANCED_FACE('',(#1103),#336,.F.) ;
#7779 = ADVANCED_FACE('',(#1104),#337,.F.) ;
#7780 = ADVANCED_FACE('',(#1105),#338,.F.) ;
#7781 = ADVANCED_FACE('',(#1106),#339,.F.) ;
#7782 = ADVANCED_FACE('',(#1107),#340,.F.) ;
#7783 = ADVANCED_FACE('',(#1108),#341,.F.) ;
#7784 = ADVANCED_FACE('',(#1109),#342,.F.) ;
#7785 = ADVANCED_FACE('',(#1110),#343,.F.) ;
#7786 = ADVANCED_FACE('',(#1111),#344,.F.) ;
#7787 = ADVANCED_FACE('',(#1112),#345,.F.) ;
#7788 = ADVANCED_FACE('',(#1113),#346,.F.) ;
#7789 = ADVANCED_FACE('',(#1114),#347,.F.) ;
#7790 = ADVANCED_FACE('',(#1115),#348,.F.) ;
#7791 = ADVANCED_FACE('',(#1116),#349,.F.) ;
#7792 = ADVANCED_FACE('',(#1117),#350,.F.) ;
#7793 = ADVANCED_FACE('',(#1118),#351,.F.) ;
#7794 = ADVANCED_FACE('',(#1119),#352,.F.) ;
#7795 = ADVANCED_FACE('',(#1120),#353,.F.) ;
#7796 = ADVANCED_FACE('',(#1121),#354,.F.) ;
#7797 = ADVANCED_FACE('',(#1122),#355,.F.) ;
#7798 = ADVANCED_FACE('',(#1123),#747,.F.) ;
#7799 = ADVANCED_FACE('',(#1124),#356,.F.) ;
#7800 = ADVANCED_FACE('',(#1125,#691),#748,.T.) ;
#7801 = ADVANCED_FACE('',(#1126),#357,.F.) ;
#7802 = ADVANCED_FACE('',(#1127),#749,.F.) ;
#7803 = ADVANCED_FACE('',(#1128),#358,.F.) ;
#7804 = ADVANCED_FACE('',(#1129),#359,.F.) ;
#7805 = ADVANCED_FACE('',(#1130),#750,.F.) ;
#7806 = ADVANCED_FACE('',(#1131),#360,.F.) ;
#7807 = ADVANCED_FACE('',(#1132),#751,.F.) ;
#7808 = ADVANCED_FACE('',(#1133),#752,.F.) ;
#7809 = ADVANCED_FACE('',(#1134),#753,.F.) ;
#7810 = ADVANCED_FACE('',(#1135),#754,.T.) ;
#7811 = ADVANCED_FACE('',(#1136,#692,#693,#694,#695,#696,#697,#698,#699),
#989,.T.) ;
#7812 = ADVANCED_FACE('',(#1137),#755,.F.) ;
#7813 = ADVANCED_FACE('',(#1138),#756,.F.) ;
#7814 = ADVANCED_FACE('',(#1139),#757,.F.) ;
#7815 = ADVANCED_FACE('',(#1140),#758,.F.) ;
#7816 = ADVANCED_FACE('',(#1141),#759,.F.) ;
#7817 = ADVANCED_FACE('',(#1142),#760,.F.) ;
#7818 = ADVANCED_FACE('',(#1143),#761,.F.) ;
#7819 = ADVANCED_FACE('',(#1144),#762,.F.) ;
#7820 = ADVANCED_FACE('',(#1145),#763,.F.) ;
#7821 = ADVANCED_FACE('',(#1146),#764,.F.) ;
#7822 = ADVANCED_FACE('',(#1147),#765,.F.) ;
#7823 = ADVANCED_FACE('',(#1148),#766,.F.) ;
#7824 = ADVANCED_FACE('',(#1149),#767,.F.) ;
#7825 = ADVANCED_FACE('',(#1150),#768,.F.) ;
#7826 = ADVANCED_FACE('',(#1151),#769,.F.) ;
#7827 = ADVANCED_FACE('',(#1152),#770,.F.) ;
#7828 = ADVANCED_FACE('',(#1153),#771,.F.) ;
#7829 = ADVANCED_FACE('',(#1154),#772,.F.) ;
#7830 = ADVANCED_FACE('',(#1155),#773,.F.) ;
#7831 = ADVANCED_FACE('',(#1156),#361,.F.) ;
#7832 = ADVANCED_FACE('',(#1157),#362,.F.) ;
#7833 = ADVANCED_FACE('',(#1158),#774,.F.) ;
#7834 = ADVANCED_FACE('',(#1159),#775,.F.) ;
#7835 = ADVANCED_FACE('',(#1160),#776,.F.) ;
#7836 = ADVANCED_FACE('',(#1161),#777,.F.) ;
#7837 = ADVANCED_FACE('',(#1162),#778,.T.) ;
#7838 = ADVANCED_FACE('',(#1163),#363,.F.) ;
#7839 = ADVANCED_FACE('',(#1164),#779,.F.) ;
#7840 = ADVANCED_FACE('',(#1165),#780,.F.) ;
#7841 = ADVANCED_FACE('',(#1166),#781,.F.) ;
#7842 = ADVANCED_FACE('',(#1167),#364,.F.) ;
#7843 = ADVANCED_FACE('',(#1168),#365,.F.) ;
#7844 = ADVANCED_FACE('',(#1169),#366,.F.) ;
#7845 = ADVANCED_FACE('',(#1170),#367,.F.) ;
#7846 = ADVANCED_FACE('',(#1171),#368,.F.) ;
#7847 = ADVANCED_FACE('',(#1172),#369,.F.) ;
#7848 = ADVANCED_FACE('',(#1173),#370,.F.) ;
#7849 = ADVANCED_FACE('',(#1174),#371,.F.) ;
#7850 = ADVANCED_FACE('',(#1175),#372,.F.) ;
#7851 = ADVANCED_FACE('',(#1176),#373,.F.) ;
#7852 = ADVANCED_FACE('',(#1177),#782,.F.) ;
#7853 = ADVANCED_FACE('',(#1178),#783,.F.) ;
#7854 = ADVANCED_FACE('',(#1179),#784,.F.) ;
#7855 = ADVANCED_FACE('',(#1180),#785,.T.) ;
#7856 = ADVANCED_FACE('',(#1181),#374,.F.) ;
#7857 = ADVANCED_FACE('',(#1182),#375,.F.) ;
#7858 = ADVANCED_FACE('',(#1183),#376,.F.) ;
#7859 = ADVANCED_FACE('',(#1184),#786,.F.) ;
#7860 = ADVANCED_FACE('',(#1185),#377,.F.) ;
#7861 = ADVANCED_FACE('',(#1186),#378,.F.) ;
#7862 = ADVANCED_FACE('',(#1187),#379,.F.) ;
#7863 = ADVANCED_FACE('',(#1188),#380,.F.) ;
#7864 = ADVANCED_FACE('',(#1189),#381,.F.) ;
#7865 = ADVANCED_FACE('',(#1190),#382,.F.) ;
#7866 = ADVANCED_FACE('',(#1191),#383,.F.) ;
#7867 = ADVANCED_FACE('',(#1192),#384,.F.) ;
#7868 = ADVANCED_FACE('',(#1193),#385,.F.) ;
#7869 = ADVANCED_FACE('',(#1194),#386,.F.) ;
#7870 = ADVANCED_FACE('',(#1195),#387,.F.) ;
#7871 = ADVANCED_FACE('',(#1196),#388,.F.) ;
#7872 = ADVANCED_FACE('',(#1197),#389,.F.) ;
#7873 = ADVANCED_FACE('',(#1198),#390,.F.) ;
#7874 = ADVANCED_FACE('',(#1199),#391,.F.) ;
#7875 = ADVANCED_FACE('',(#1200),#392,.F.) ;
#7876 = ADVANCED_FACE('',(#1201),#393,.F.) ;
#7877 = ADVANCED_FACE('',(#1202),#394,.F.) ;
#7878 = ADVANCED_FACE('',(#1203),#395,.F.) ;
#7879 = ADVANCED_FACE('',(#1204),#396,.F.) ;
#7880 = ADVANCED_FACE('',(#1205),#397,.F.) ;
#7881 = ADVANCED_FACE('',(#1206),#398,.F.) ;
#7882 = ADVANCED_FACE('',(#1207),#399,.F.) ;
#7883 = ADVANCED_FACE('',(#1208),#400,.F.) ;
#7884 = ADVANCED_FACE('',(#1209),#401,.F.) ;
#7885 = ADVANCED_FACE('',(#1210),#402,.F.) ;
#7886 = ADVANCED_FACE('',(#1211),#403,.F.) ;
#7887 = ADVANCED_FACE('',(#1212),#404,.F.) ;
#7888 = ADVANCED_FACE('',(#1213),#405,.F.) ;
#7889 = ADVANCED_FACE('',(#1214),#787,.F.) ;
#7890 = ADVANCED_FACE('',(#1215),#406,.F.) ;
#7891 = ADVANCED_FACE('',(#1216),#788,.T.) ;
#7892 = ADVANCED_FACE('',(#1217),#789,.F.) ;
#7893 = ADVANCED_FACE('',(#1218),#790,.F.) ;
#7894 = ADVANCED_FACE('',(#1219),#791,.F.) ;
#7895 = ADVANCED_FACE('',(#1220),#792,.F.) ;
#7896 = ADVANCED_FACE('',(#1221),#793,.F.) ;
#7897 = ADVANCED_FACE('',(#1222),#794,.F.) ;
#7898 = ADVANCED_FACE('',(#1223),#795,.F.) ;
#7899 = ADVANCED_FACE('',(#1224),#796,.F.) ;
#7900 = ADVANCED_FACE('',(#1225),#797,.F.) ;
#7901 = ADVANCED_FACE('',(#1226),#407,.F.) ;
#7902 = ADVANCED_FACE('',(#1227),#408,.F.) ;
#7903 = ADVANCED_FACE('',(#1228),#798,.F.) ;
#7904 = ADVANCED_FACE('',(#1229),#799,.F.) ;
#7905 = ADVANCED_FACE('',(#1230),#800,.F.) ;
#7906 = ADVANCED_FACE('',(#1231),#801,.F.) ;
#7907 = ADVANCED_FACE('',(#1232),#802,.T.) ;
#7908 = ADVANCED_FACE('',(#1233),#990,.T.) ;
#7909 = ADVANCED_FACE('',(#1234,#700),#803,.F.) ;
#7910 = ADVANCED_FACE('',(#1235,#701),#804,.F.) ;
#7911 = ADVANCED_FACE('',(#1236),#991,.T.) ;
#7912 = ADVANCED_FACE('',(#1237),#7721,.F.) ;
#7913 = ADVANCED_FACE('',(#1238),#409,.T.) ;
#7914 = ADVANCED_FACE('',(#1239),#316,.F.) ;
#7915 = ADVANCED_FACE('',(#1240),#992,.F.) ;
#7916 = ADVANCED_FACE('',(#1241),#7722,.F.) ;
#7917 = ADVANCED_FACE('',(#1242),#410,.T.) ;
#7918 = ADVANCED_FACE('',(#1243),#993,.F.) ;
#7919 = ADVANCED_FACE('',(#1244),#7723,.F.) ;
#7920 = ADVANCED_FACE('',(#1245),#411,.T.) ;
#7921 = ADVANCED_FACE('',(#1246),#994,.F.) ;
#7922 = ADVANCED_FACE('',(#1247),#7724,.F.) ;
#7923 = ADVANCED_FACE('',(#1248),#412,.T.) ;
#7924 = ADVANCED_FACE('',(#1249),#995,.F.) ;
#7925 = ADVANCED_FACE('',(#1250,#702),#805,.T.) ;
#7926 = ADVANCED_FACE('',(#1251,#703),#806,.T.) ;
#7927 = ADVANCED_FACE('',(#1252,#704),#807,.T.) ;
#7928 = ADVANCED_FACE('',(#1253,#705),#808,.T.) ;
#7929 = ADVANCED_FACE('',(#1254),#996,.F.) ;
#7930 = ADVANCED_FACE('',(#1255),#997,.F.) ;
#7931 = ADVANCED_FACE('',(#1256),#998,.F.) ;
#7932 = ADVANCED_FACE('',(#1257),#999,.F.) ;
#7933 = ADVANCED_FACE('',(#1258),#1000,.F.) ;
#7934 = ADVANCED_FACE('',(#1259),#1001,.F.) ;
#7935 = ADVANCED_FACE('',(#1260),#1002,.F.) ;
#7936 = ADVANCED_FACE('',(#1261),#1003,.F.) ;
#7937 = ADVANCED_FACE('',(#1262,#706),#809,.T.) ;
#7938 = ADVANCED_FACE('',(#1263),#1004,.F.) ;
#7939 = ADVANCED_FACE('',(#1264),#1005,.F.) ;
#7940 = ADVANCED_FACE('',(#1265),#1006,.F.) ;
#7941 = ADVANCED_FACE('',(#1266),#1007,.F.) ;
#7942 = ADVANCED_FACE('',(#1267,#707),#810,.T.) ;
#7943 = ADVANCED_FACE('',(#1268),#1008,.T.) ;
#7944 = ADVANCED_FACE('',(#1269,#708),#811,.F.) ;
#7945 = ADVANCED_FACE('',(#1270),#1009,.F.) ;
#7946 = ADVANCED_FACE('',(#1271,#709),#812,.F.) ;
#7947 = ADVANCED_FACE('',(#1272),#1010,.F.) ;
#7948 = ADVANCED_FACE('',(#1273,#710),#813,.F.) ;
#7949 = ADVANCED_FACE('',(#1274),#1011,.F.) ;
#7950 = ADVANCED_FACE('',(#1275,#711),#814,.F.) ;
#7951 = ADVANCED_FACE('',(#1276),#1012,.F.) ;
#7952 = ADVANCED_FACE('',(#1277,#712),#815,.T.) ;
#7953 = ADVANCED_FACE('',(#1278),#1013,.F.) ;
#7954 = ADVANCED_FACE('',(#1279,#713,#714,#715,#716,#717),#816,.T.) ;
#7955 = ADVANCED_FACE('',(#1280),#7725,.T.) ;
#7956 = ADVANCED_FACE('',(#1281),#1014,.T.) ;
#7957 = ADVANCED_FACE('',(#1282),#7726,.T.) ;
#7958 = ADVANCED_FACE('',(#1283),#7727,.T.) ;
#7959 = ADVANCED_FACE('',(#1284,#718),#817,.T.) ;
#7960 = ADVANCED_FACE('',(#1285),#1015,.F.) ;
#7961 = ADVANCED_FACE('',(#1286),#818,.F.) ;
#7962 = ADVANCED_FACE('',(#1287),#819,.F.) ;
#7963 = ADVANCED_FACE('',(#1288),#820,.F.) ;
#7964 = ADVANCED_FACE('',(#1289),#821,.T.) ;
#7965 = ADVANCED_FACE('',(#1290),#822,.F.) ;
#7966 = ADVANCED_FACE('',(#1291),#823,.F.) ;
#7967 = ADVANCED_FACE('',(#1292),#824,.F.) ;
#7968 = ADVANCED_FACE('',(#1293),#825,.T.) ;
#7969 = ADVANCED_FACE('',(#1294),#826,.F.) ;
#7970 = ADVANCED_FACE('',(#1295),#827,.F.) ;
#7971 = ADVANCED_FACE('',(#1296),#828,.F.) ;
#7972 = ADVANCED_FACE('',(#1297),#829,.T.) ;
#7973 = ADVANCED_FACE('',(#1298),#830,.F.) ;
#7974 = ADVANCED_FACE('',(#1299),#831,.F.) ;
#7975 = ADVANCED_FACE('',(#1300),#832,.F.) ;
#7976 = ADVANCED_FACE('',(#1301),#833,.T.) ;
#7977 = ADVANCED_FACE('',(#1302,#719,#720,#721,#722),#1016,.F.) ;
#7978 = ADVANCED_FACE('',(#1303,#723),#834,.T.) ;
#7979 = ADVANCED_FACE('',(#1304,#724,#725,#726,#727),#1017,.T.) ;
#7980 = ADVANCED_FACE('',(#1305,#728),#835,.T.) ;
#7981 = ADVANCED_FACE('',(#1306),#315,.T.) ;
#7982 = ADVANCED_FACE('',(#1307),#1018,.T.) ;
#7983 = ADVANCED_FACE('',(#1308),#1019,.T.) ;
#7984 = ADVANCED_FACE('',(#1309),#1020,.T.) ;
#7985 = ADVANCED_FACE('',(#1310),#1021,.T.) ;
#7986 = ADVANCED_FACE('',(#1311),#1022,.T.) ;
#7987 = ADVANCED_FACE('',(#1312),#1023,.T.) ;
#7988 = ADVANCED_FACE('',(#1313),#1024,.T.) ;
#7989 = ADVANCED_FACE('',(#1314),#1025,.T.) ;
#7990 = ADVANCED_FACE('',(#1315),#1026,.T.) ;
#7991 = ADVANCED_FACE('',(#1316),#1027,.T.) ;
#7992 = ADVANCED_FACE('',(#1317),#1028,.T.) ;
#7993 = ADVANCED_FACE('',(#1318),#1029,.T.) ;
#7994 = ADVANCED_FACE('',(#1319),#1030,.T.) ;
#7995 = ADVANCED_FACE('',(#1320),#1031,.T.) ;
#7996 = ADVANCED_FACE('',(#1321),#1032,.T.) ;
#7997 = ADVANCED_FACE('',(#1322),#1033,.T.) ;
#7998 = ADVANCED_FACE('',(#1323),#1034,.T.) ;
#7999 = ADVANCED_FACE('',(#1324),#1035,.T.) ;
#8000 = ADVANCED_FACE('',(#1325),#1036,.T.) ;
#8001 = ADVANCED_FACE('',(#1326),#1037,.T.) ;
#8002 = ADVANCED_FACE('',(#1327),#1038,.T.) ;
#8003 = ADVANCED_FACE('',(#1328),#1039,.T.) ;
#8004 = ADVANCED_FACE('',(#1329),#1040,.T.) ;
#8005 = ADVANCED_FACE('',(#1330),#1041,.T.) ;
#8006 = ADVANCED_FACE('',(#1331),#1042,.T.) ;
#8007 = ADVANCED_FACE('',(#1332),#1043,.T.) ;
#8008 = ADVANCED_FACE('',(#1333),#1044,.T.) ;
#8009 = ADVANCED_FACE('',(#1334),#836,.T.) ;
#8010 = ADVANCED_FACE('',(#1335),#413,.F.) ;
#8011 = ADVANCED_FACE('',(#1336),#837,.F.) ;
#8012 = ADVANCED_FACE('',(#1337),#1045,.T.) ;
#8013 = ADVANCED_FACE('',(#1338),#414,.F.) ;
#8014 = ADVANCED_FACE('',(#1339),#317,.F.) ;
#8015 = ADVANCED_FACE('',(#1340),#1046,.T.) ;
#8016 = ADVANCED_FACE('',(#1341,#729),#838,.F.) ;
#8017 = ADVANCED_FACE('',(#1342),#7728,.T.) ;
#8018 = ADVANCED_FACE('',(#1343),#839,.F.) ;
#8019 = ADVANCED_FACE('',(#1344),#840,.F.) ;
#8020 = ADVANCED_FACE('',(#1345),#841,.F.) ;
#8021 = ADVANCED_FACE('',(#1346),#842,.F.) ;
#8022 = ADVANCED_FACE('',(#1347),#1047,.T.) ;
#8023 = ADVANCED_FACE('',(#1348),#843,.F.) ;
#8024 = ADVANCED_FACE('',(#1349),#844,.F.) ;
#8025 = ADVANCED_FACE('',(#1350),#845,.F.) ;
#8026 = ADVANCED_FACE('',(#1351),#846,.F.) ;
#8027 = ADVANCED_FACE('',(#1352),#847,.F.) ;
#8028 = ADVANCED_FACE('',(#1353),#848,.F.) ;
#8029 = ADVANCED_FACE('',(#1354),#849,.F.) ;
#8030 = ADVANCED_FACE('',(#1355),#850,.F.) ;
#8031 = ADVANCED_FACE('',(#1356),#851,.F.) ;
#8032 = ADVANCED_FACE('',(#1357),#852,.F.) ;
#8033 = ADVANCED_FACE('',(#1358),#853,.F.) ;
#8034 = ADVANCED_FACE('',(#1359),#854,.F.) ;
#8035 = ADVANCED_FACE('',(#1360),#855,.F.) ;
#8036 = ADVANCED_FACE('',(#1361),#856,.F.) ;
#8037 = ADVANCED_FACE('',(#1362),#857,.F.) ;
#8038 = ADVANCED_FACE('',(#1363),#858,.F.) ;
#8039 = ADVANCED_FACE('',(#1364),#859,.F.) ;
#8040 = ADVANCED_FACE('',(#1365),#860,.F.) ;
#8041 = ADVANCED_FACE('',(#1366),#861,.F.) ;
#8042 = ADVANCED_FACE('',(#1367),#862,.F.) ;
#8043 = ADVANCED_FACE('',(#1368),#863,.F.) ;
#8044 = ADVANCED_FACE('',(#1369),#864,.F.) ;
#8045 = ADVANCED_FACE('',(#1370),#865,.F.) ;
#8046 = ADVANCED_FACE('',(#1371),#866,.F.) ;
#8047 = ADVANCED_FACE('',(#1372),#867,.F.) ;
#8048 = ADVANCED_FACE('',(#1373),#868,.F.) ;
#8049 = ADVANCED_FACE('',(#1374),#869,.F.) ;
#8050 = ADVANCED_FACE('',(#1375),#870,.F.) ;
#8051 = ADVANCED_FACE('',(#1376),#871,.F.) ;
#8052 = ADVANCED_FACE('',(#1377),#872,.F.) ;
#8053 = ADVANCED_FACE('',(#1378),#873,.F.) ;
#8054 = ADVANCED_FACE('',(#1379),#874,.F.) ;
#8055 = ADVANCED_FACE('',(#1380),#875,.F.) ;
#8056 = ADVANCED_FACE('',(#1381),#876,.F.) ;
#8057 = ADVANCED_FACE('',(#1382),#877,.F.) ;
#8058 = ADVANCED_FACE('',(#1383),#878,.F.) ;
#8059 = ADVANCED_FACE('',(#1384),#879,.F.) ;
#8060 = ADVANCED_FACE('',(#1385),#880,.F.) ;
#8061 = ADVANCED_FACE('',(#1386),#881,.F.) ;
#8062 = ADVANCED_FACE('',(#1387),#882,.F.) ;
#8063 = ADVANCED_FACE('',(#1388),#883,.F.) ;
#8064 = ADVANCED_FACE('',(#1389),#884,.F.) ;
#8065 = ADVANCED_FACE('',(#1390),#885,.F.) ;
#8066 = ADVANCED_FACE('',(#1391),#886,.F.) ;
#8067 = ADVANCED_FACE('',(#1392),#887,.F.) ;
#8068 = ADVANCED_FACE('',(#1393),#888,.F.) ;
#8069 = ADVANCED_FACE('',(#1394),#889,.F.) ;
#8070 = ADVANCED_FACE('',(#1395),#890,.F.) ;
#8071 = ADVANCED_FACE('',(#1396),#891,.F.) ;
#8072 = ADVANCED_FACE('',(#1397),#892,.F.) ;
#8073 = ADVANCED_FACE('',(#1398),#893,.F.) ;
#8074 = ADVANCED_FACE('',(#1399),#894,.F.) ;
#8075 = ADVANCED_FACE('',(#1400),#895,.F.) ;
#8076 = ADVANCED_FACE('',(#1401),#896,.F.) ;
#8077 = ADVANCED_FACE('',(#1402),#897,.F.) ;
#8078 = ADVANCED_FACE('',(#1403),#898,.F.) ;
#8079 = ADVANCED_FACE('',(#1404),#899,.F.) ;
#8080 = ADVANCED_FACE('',(#1405),#900,.F.) ;
#8081 = ADVANCED_FACE('',(#1406),#901,.F.) ;
#8082 = ADVANCED_FACE('',(#1407),#902,.F.) ;
#8083 = ADVANCED_FACE('',(#1408),#903,.F.) ;
#8084 = ADVANCED_FACE('',(#1409),#904,.F.) ;
#8085 = ADVANCED_FACE('',(#1410),#905,.F.) ;
#8086 = ADVANCED_FACE('',(#1411),#906,.F.) ;
#8087 = ADVANCED_FACE('',(#1412),#907,.F.) ;
#8088 = ADVANCED_FACE('',(#1413),#908,.F.) ;
#8089 = ADVANCED_FACE('',(#1414),#909,.F.) ;
#8090 = ADVANCED_FACE('',(#1415),#910,.F.) ;
#8091 = ADVANCED_FACE('',(#1416),#911,.F.) ;
#8092 = ADVANCED_FACE('',(#1417),#912,.F.) ;
#8093 = ADVANCED_FACE('',(#1418),#913,.F.) ;
#8094 = ADVANCED_FACE('',(#1419),#914,.F.) ;
#8095 = ADVANCED_FACE('',(#1420),#915,.F.) ;
#8096 = ADVANCED_FACE('',(#1421),#916,.F.) ;
#8097 = ADVANCED_FACE('',(#1422),#917,.F.) ;
#8098 = ADVANCED_FACE('',(#1423),#918,.F.) ;
#8099 = ADVANCED_FACE('',(#1424),#919,.F.) ;
#8100 = ADVANCED_FACE('',(#1425),#920,.F.) ;
#8101 = ADVANCED_FACE('',(#1426),#921,.F.) ;
#8102 = ADVANCED_FACE('',(#1427),#922,.F.) ;
#8103 = ADVANCED_FACE('',(#1428),#923,.F.) ;
#8104 = ADVANCED_FACE('',(#1429),#924,.F.) ;
#8105 = ADVANCED_FACE('',(#1430),#925,.F.) ;
#8106 = ADVANCED_FACE('',(#1431),#926,.F.) ;
#8107 = ADVANCED_FACE('',(#1432),#927,.F.) ;
#8108 = ADVANCED_FACE('',(#1433),#928,.F.) ;
#8109 = ADVANCED_FACE('',(#1434),#929,.F.) ;
#8110 = ADVANCED_FACE('',(#1435),#930,.F.) ;
#8111 = ADVANCED_FACE('',(#1436),#931,.F.) ;
#8112 = ADVANCED_FACE('',(#1437),#932,.F.) ;
#8113 = ADVANCED_FACE('',(#1438),#933,.F.) ;
#8114 = ADVANCED_FACE('',(#1439),#934,.F.) ;
#8115 = ADVANCED_FACE('',(#1440),#935,.F.) ;
#8116 = ADVANCED_FACE('',(#1441),#936,.F.) ;
#8117 = ADVANCED_FACE('',(#1442),#937,.F.) ;
#8118 = ADVANCED_FACE('',(#1443),#938,.F.) ;
#8119 = ADVANCED_FACE('',(#1444),#939,.F.) ;
#8120 = ADVANCED_FACE('',(#1445),#940,.F.) ;
#8121 = ADVANCED_FACE('',(#1446),#941,.F.) ;
#8122 = ADVANCED_FACE('',(#1447),#942,.F.) ;
#8123 = ADVANCED_FACE('',(#1448),#943,.F.) ;
#8124 = ADVANCED_FACE('',(#1449),#944,.F.) ;
#8125 = ADVANCED_FACE('',(#1450),#945,.F.) ;
#8126 = ADVANCED_FACE('',(#1451),#946,.F.) ;
#8127 = ADVANCED_FACE('',(#1452),#947,.F.) ;
#8128 = ADVANCED_FACE('',(#1453),#318,.T.) ;
#8129 = ADVANCED_FACE('',(#1454),#7729,.T.) ;
#8130 = ADVANCED_FACE('',(#1455,#730),#948,.T.) ;
#8131 = ADVANCED_FACE('',(#1456),#7730,.F.) ;
#8132 = ADVANCED_FACE('',(#1457),#1048,.T.) ;
#8133 = ADVANCED_FACE('',(#1458),#1049,.T.) ;
#8134 = ADVANCED_FACE('',(#1459),#1050,.T.) ;
#8135 = ADVANCED_FACE('',(#1460),#1051,.T.) ;
#8136 = ADVANCED_FACE('',(#1461),#1052,.T.) ;
#8137 = ADVANCED_FACE('',(#1462),#1053,.T.) ;
#8138 = ADVANCED_FACE('',(#1463),#949,.F.) ;
#8139 = ADVANCED_FACE('',(#1464),#950,.F.) ;
#8140 = ADVANCED_FACE('',(#1465),#951,.F.) ;
#8141 = ADVANCED_FACE('',(#1466),#952,.T.) ;
#8142 = ADVANCED_FACE('',(#1467),#953,.T.) ;
#8143 = ADVANCED_FACE('',(#1468),#954,.T.) ;
#8144 = ADVANCED_FACE('',(#1469),#955,.T.) ;
#8145 = ADVANCED_FACE('',(#1470),#956,.T.) ;
#8146 = ADVANCED_FACE('',(#1471),#957,.T.) ;
#8147 = ADVANCED_FACE('',(#1472),#958,.F.) ;
#8148 = ADVANCED_FACE('',(#1473),#959,.F.) ;
#8149 = ADVANCED_FACE('',(#1474),#960,.F.) ;
#8150 = ADVANCED_FACE('',(#1475),#961,.F.) ;
#8151 = ADVANCED_FACE('',(#1476),#962,.F.) ;
#8152 = ADVANCED_FACE('',(#1477),#963,.F.) ;
#8153 = ADVANCED_FACE('',(#1478),#7731,.F.) ;
#8154 = ADVANCED_FACE('',(#1479),#964,.F.) ;
#8155 = ADVANCED_FACE('',(#1480),#965,.F.) ;
#8156 = ADVANCED_FACE('',(#1481),#966,.F.) ;
#8157 = ADVANCED_FACE('',(#1482,#731),#967,.T.) ;
#8158 = ADVANCED_FACE('',(#1483),#1054,.T.) ;
#8159 = ADVANCED_FACE('',(#1484,#732),#968,.T.) ;
#8160 = ADVANCED_FACE('',(#1485),#7732,.F.) ;
#8161 = ADVANCED_FACE('',(#1486),#1055,.F.) ;
#8162 = ADVANCED_FACE('',(#1487),#7733,.F.) ;
#8163 = ADVANCED_FACE('',(#1488),#7734,.F.) ;
#8164 = ADVANCED_FACE('',(#1489),#1056,.F.) ;
#8165 = ADVANCED_FACE('',(#1490),#7735,.F.) ;
#8166 = ADVANCED_FACE('',(#1491),#1057,.F.) ;
#8167 = ADVANCED_FACE('',(#1492),#969,.T.) ;
#8168 = ADVANCED_FACE('',(#1493),#970,.T.) ;
#8169 = ADVANCED_FACE('',(#1494),#971,.F.) ;
#8170 = ADVANCED_FACE('',(#1495,#733,#734),#972,.T.) ;
#8171 = ADVANCED_FACE('',(#1496),#1058,.F.) ;
#8172 = ADVANCED_FACE('',(#1497),#973,.T.) ;
#8173 = ADVANCED_FACE('',(#1498),#974,.T.) ;
#8174 = ADVANCED_FACE('',(#1499),#1059,.F.) ;
#8175 = ADVANCED_FACE('',(#1500),#975,.F.) ;
#8176 = ADVANCED_FACE('',(#1501),#1060,.T.) ;
#8177 = ADVANCED_FACE('',(#1502,#735,#736),#976,.F.) ;
#8178 = CLOSED_SHELL('',(#7736,#7737,#7738,#7739,#7740,#7741,#7742,#7743,
#7744,#7745,#7746,#7747,#7748,#7749,#7750,#7751,#7752,#7753,#7754,#7755,
#7756,#7757,#7758,#7759,#7760,#7761,#7762,#7763,#7764,#7765,#7766,#7767,
#7768,#7769,#7770,#7771)) ;
#8179 = CLOSED_SHELL('',(#7772,#7773,#7774,#7775,#7776,#7777,#7778,#7779,
#7780,#7781,#7782,#7783,#7784,#7785,#7786,#7787,#7788,#7789,#7790,#7791,
#7792,#7793,#7794,#7795,#7796,#7797,#7798,#7799,#7800,#7801,#7802,#7803,
#7804,#7805,#7806,#7807,#7808,#7809,#7810,#7811,#7812,#7813,#7814,#7815,
#7816,#7817,#7818,#7819,#7820,#7821,#7822,#7823,#7824,#7825,#7826,#7827,
#7828,#7829,#7830,#7831,#7832,#7833,#7834,#7835,#7836,#7837,#7838,#7839,
#7840,#7841,#7842,#7843,#7844,#7845,#7846,#7847,#7848,#7849,#7850,#7851,
#7852,#7853,#7854,#7855,#7856,#7857,#7858,#7859,#7860,#7861,#7862,#7863,
#7864,#7865,#7866,#7867,#7868,#7869,#7870,#7871,#7872,#7873,#7874,#7875,
#7876,#7877,#7878,#7879,#7880,#7881,#7882,#7883,#7884,#7885,#7886,#7887,
#7888,#7889,#7890,#7891,#7892,#7893,#7894,#7895,#7896,#7897,#7898,#7899,
#7900,#7901,#7902,#7903,#7904,#7905,#7906,#7907,#7908,#7909,#7910,#7911,
#7912,#7913,#7914,#7915,#7916,#7917,#7918,#7919,#7920,#7921,#7922,#7923,
#7924,#7925,#7926,#7927,#7928,#7929,#7930,#7931,#7932,#7933,#7934,#7935,
#7936,#7937,#7938,#7939,#7940,#7941,#7942,#7943,#7944,#7945,#7946,#7947,
#7948,#7949,#7950,#7951,#7952,#7953,#7954,#7955,#7956,#7957,#7958,#7959,
#7960)) ;
#8180 = CLOSED_SHELL('',(#7961,#7962,#7963,#7964,#7965,#7966,#7967,#7968,
#7969,#7970,#7971,#7972,#7973,#7974,#7975,#7976,#7977,#7978,#7979,#7980)) ;
#8181 = CLOSED_SHELL('',(#7981)) ;
#8182 = CLOSED_SHELL('',(#7982,#7983,#7984,#7985,#7986,#7987,#7988,#7989,
#7990,#7991,#7992,#7993,#7994,#7995,#7996,#7997,#7998,#7999,#8000,#8001,
#8002,#8003,#8004,#8005,#8006,#8007,#8008,#8009,#8010,#8011,#8012,#8013,
#8014,#8015,#8016,#8017,#8018,#8019,#8020,#8021,#8022,#8023,#8024,#8025,
#8026,#8027,#8028,#8029,#8030,#8031,#8032,#8033,#8034,#8035,#8036,#8037,
#8038,#8039,#8040,#8041,#8042,#8043,#8044,#8045,#8046,#8047,#8048,#8049,
#8050,#8051,#8052,#8053,#8054,#8055,#8056,#8057,#8058,#8059,#8060,#8061,
#8062,#8063,#8064,#8065,#8066,#8067,#8068,#8069,#8070,#8071,#8072,#8073,
#8074,#8075,#8076,#8077,#8078,#8079,#8080,#8081,#8082,#8083,#8084,#8085,
#8086,#8087,#8088,#8089,#8090,#8091,#8092,#8093,#8094,#8095,#8096,#8097,
#8098,#8099,#8100,#8101,#8102,#8103,#8104,#8105,#8106,#8107,#8108,#8109,
#8110,#8111,#8112,#8113,#8114,#8115,#8116,#8117,#8118,#8119,#8120,#8121,
#8122,#8123,#8124,#8125,#8126,#8127,#8128,#8129,#8130,#8131,#8132,#8133,
#8134,#8135,#8136,#8137,#8138,#8139,#8140,#8141,#8142,#8143,#8144,#8145,
#8146,#8147,#8148,#8149,#8150,#8151,#8152,#8153,#8154,#8155,#8156)) ;
#8183 = CLOSED_SHELL('',(#8157,#8158,#8159,#8160,#8161,#8162,#8163,#8164,
#8165)) ;
#8184 = CLOSED_SHELL('',(#8166,#8167,#8168,#8169,#8170,#8171,#8172,#8173,
#8174,#8175,#8176,#8177)) ;
#8185 = DERIVED_UNIT_ELEMENT(#8199,1.) ;
#8186 = DERIVED_UNIT_ELEMENT(#16944,-3.) ;
#8187 = DERIVED_UNIT_ELEMENT(#8199,1.) ;
#8188 = DERIVED_UNIT_ELEMENT(#16944,-3.) ;
#8189 = DERIVED_UNIT_ELEMENT(#8199,1.) ;
#8190 = DERIVED_UNIT_ELEMENT(#16944,-3.) ;
#8191 = DERIVED_UNIT_ELEMENT(#8199,1.) ;
#8192 = DERIVED_UNIT_ELEMENT(#16944,-3.) ;
#8193 = DERIVED_UNIT_ELEMENT(#8199,1.) ;
#8194 = DERIVED_UNIT_ELEMENT(#16944,-3.) ;
#8195 = DERIVED_UNIT_ELEMENT(#8199,1.) ;
#8196 = DERIVED_UNIT_ELEMENT(#16944,-3.) ;
#8197 = DERIVED_UNIT_ELEMENT(#8199,1.) ;
#8198 = DERIVED_UNIT_ELEMENT(#16944,-3.) ;
#8199 = (
MASS_UNIT()
NAMED_UNIT(*)
SI_UNIT(.KILO.,.GRAM.)
) ;
#8200 = DERIVED_UNIT((#8185,#8186)) ;
#8201 = DERIVED_UNIT((#8187,#8188)) ;
#8202 = DERIVED_UNIT((#8189,#8190)) ;
#8203 = DERIVED_UNIT((#8191,#8192)) ;
#8204 = DERIVED_UNIT((#8193,#8194)) ;
#8205 = DERIVED_UNIT((#8195,#8196)) ;
#8206 = DERIVED_UNIT((#8197,#8198)) ;
#8207 = MEASURE_REPRESENTATION_ITEM('density measure',
POSITIVE_RATIO_MEASURE(7850.),#8200) ;
#8208 = MEASURE_REPRESENTATION_ITEM('density measure',
POSITIVE_RATIO_MEASURE(7850.),#8201) ;
#8209 = MEASURE_REPRESENTATION_ITEM('density measure',
POSITIVE_RATIO_MEASURE(7850.),#8202) ;
#8210 = MEASURE_REPRESENTATION_ITEM('density measure',
POSITIVE_RATIO_MEASURE(7850.),#8203) ;
#8211 = MEASURE_REPRESENTATION_ITEM('density measure',
POSITIVE_RATIO_MEASURE(7850.),#8204) ;
#8212 = MEASURE_REPRESENTATION_ITEM('density measure',
POSITIVE_RATIO_MEASURE(7850.),#8205) ;
#8213 = MEASURE_REPRESENTATION_ITEM('density measure',
POSITIVE_RATIO_MEASURE(7850.),#8206) ;
#8214 = PROPERTY_DEFINITION_REPRESENTATION(#8249,#8228) ;
#8215 = PROPERTY_DEFINITION_REPRESENTATION(#8250,#8229) ;
#8216 = PROPERTY_DEFINITION_REPRESENTATION(#8251,#8230) ;
#8217 = PROPERTY_DEFINITION_REPRESENTATION(#8252,#8231) ;
#8218 = PROPERTY_DEFINITION_REPRESENTATION(#8253,#8232) ;
#8219 = PROPERTY_DEFINITION_REPRESENTATION(#8254,#8233) ;
#8220 = PROPERTY_DEFINITION_REPRESENTATION(#8255,#8234) ;
#8221 = PROPERTY_DEFINITION_REPRESENTATION(#8256,#8235) ;
#8222 = PROPERTY_DEFINITION_REPRESENTATION(#8257,#8236) ;
#8223 = PROPERTY_DEFINITION_REPRESENTATION(#8258,#8237) ;
#8224 = PROPERTY_DEFINITION_REPRESENTATION(#8259,#8238) ;
#8225 = PROPERTY_DEFINITION_REPRESENTATION(#8260,#8239) ;
#8226 = PROPERTY_DEFINITION_REPRESENTATION(#8261,#8240) ;
#8227 = PROPERTY_DEFINITION_REPRESENTATION(#8262,#8241) ;
#8228 = REPRESENTATION('material name',(#8242),#16935) ;
#8229 = REPRESENTATION('density',(#8207),#16935) ;
#8230 = REPRESENTATION('material name',(#8243),#16936) ;
#8231 = REPRESENTATION('density',(#8208),#16936) ;
#8232 = REPRESENTATION('material name',(#8244),#16937) ;
#8233 = REPRESENTATION('density',(#8209),#16937) ;
#8234 = REPRESENTATION('material name',(#8245),#16938) ;
#8235 = REPRESENTATION('density',(#8210),#16938) ;
#8236 = REPRESENTATION('material name',(#8246),#16939) ;
#8237 = REPRESENTATION('density',(#8211),#16939) ;
#8238 = REPRESENTATION('material name',(#8247),#16940) ;
#8239 = REPRESENTATION('density',(#8212),#16940) ;
#8240 = REPRESENTATION('material name',(#8248),#16941) ;
#8241 = REPRESENTATION('density',(#8213),#16941) ;
#8242 = DESCRIPTIVE_REPRESENTATION_ITEM('Steel','Steel') ;
#8243 = DESCRIPTIVE_REPRESENTATION_ITEM('Steel','Steel') ;
#8244 = DESCRIPTIVE_REPRESENTATION_ITEM('Steel','Steel') ;
#8245 = DESCRIPTIVE_REPRESENTATION_ITEM('Steel','Steel') ;
#8246 = DESCRIPTIVE_REPRESENTATION_ITEM('Steel','Steel') ;
#8247 = DESCRIPTIVE_REPRESENTATION_ITEM('Steel','Steel') ;
#8248 = DESCRIPTIVE_REPRESENTATION_ITEM('Steel','Steel') ;
#8249 = PROPERTY_DEFINITION('material property','material name',#17028) ;
#8250 = PROPERTY_DEFINITION('material property','density of part',#17028) ;
#8251 = PROPERTY_DEFINITION('material property','material name',#17029) ;
#8252 = PROPERTY_DEFINITION('material property','density of part',#17029) ;
#8253 = PROPERTY_DEFINITION('material property','material name',#17030) ;
#8254 = PROPERTY_DEFINITION('material property','density of part',#17030) ;
#8255 = PROPERTY_DEFINITION('material property','material name',#17031) ;
#8256 = PROPERTY_DEFINITION('material property','density of part',#17031) ;
#8257 = PROPERTY_DEFINITION('material property','material name',#17032) ;
#8258 = PROPERTY_DEFINITION('material property','density of part',#17032) ;
#8259 = PROPERTY_DEFINITION('material property','material name',#17033) ;
#8260 = PROPERTY_DEFINITION('material property','density of part',#17033) ;
#8261 = PROPERTY_DEFINITION('material property','material name',#17034) ;
#8262 = PROPERTY_DEFINITION('material property','density of part',#17034) ;
#8263 = AXIS2_PLACEMENT_3D('',#10952,#8972,#8973) ;
#8264 = AXIS2_PLACEMENT_3D('',#10953,#8974,#8975) ;
#8265 = AXIS2_PLACEMENT_3D('',#10954,#8976,#8977) ;
#8266 = AXIS2_PLACEMENT_3D('',#10956,#8978,#8979) ;
#8267 = AXIS2_PLACEMENT_3D('',#10959,#8981,#8982) ;
#8268 = AXIS2_PLACEMENT_3D('',#10960,#8983,#8984) ;
#8269 = AXIS2_PLACEMENT_3D('',#10964,#8986,#8987) ;
#8270 = AXIS2_PLACEMENT_3D('',#10965,#8988,#8989) ;
#8271 = AXIS2_PLACEMENT_3D('',#10966,#8990,#8991) ;
#8272 = AXIS2_PLACEMENT_3D('',#10968,#8992,#8993) ;
#8273 = AXIS2_PLACEMENT_3D('',#10969,#8994,#8995) ;
#8274 = AXIS2_PLACEMENT_3D('',#10972,#8997,#8998) ;
#8275 = AXIS2_PLACEMENT_3D('',#10974,#8999,#9000) ;
#8276 = AXIS2_PLACEMENT_3D('',#10977,#9002,#9003) ;
#8277 = AXIS2_PLACEMENT_3D('',#10978,#9004,#9005) ;
#8278 = AXIS2_PLACEMENT_3D('',#10982,#9007,#9008) ;
#8279 = AXIS2_PLACEMENT_3D('',#10983,#9009,#9010) ;
#8280 = AXIS2_PLACEMENT_3D('',#10984,#9011,#9012) ;
#8281 = AXIS2_PLACEMENT_3D('',#10986,#9013,#9014) ;
#8282 = AXIS2_PLACEMENT_3D('',#10987,#9015,#9016) ;
#8283 = AXIS2_PLACEMENT_3D('',#10990,#9018,#9019) ;
#8284 = AXIS2_PLACEMENT_3D('',#10993,#9020,#9021) ;
#8285 = AXIS2_PLACEMENT_3D('',#10996,#9023,#9024) ;
#8286 = AXIS2_PLACEMENT_3D('',#10997,#9025,#9026) ;
#8287 = AXIS2_PLACEMENT_3D('',#11003,#9030,#9031) ;
#8288 = AXIS2_PLACEMENT_3D('',#11005,#9032,#9033) ;
#8289 = AXIS2_PLACEMENT_3D('',#11006,#9034,#9035) ;
#8290 = AXIS2_PLACEMENT_3D('',#11007,#9036,#9037) ;
#8291 = AXIS2_PLACEMENT_3D('',#11010,#9038,#9039) ;
#8292 = AXIS2_PLACEMENT_3D('',#11012,#9041,#9042) ;
#8293 = AXIS2_PLACEMENT_3D('',#11018,#9046,#9047) ;
#8294 = AXIS2_PLACEMENT_3D('',#11019,#9048,#9049) ;
#8295 = AXIS2_PLACEMENT_3D('',#11020,#9050,#9051) ;
#8296 = AXIS2_PLACEMENT_3D('',#11030,#9052,#9053) ;
#8297 = AXIS2_PLACEMENT_3D('',#11050,#9055,#9056) ;
#8298 = AXIS2_PLACEMENT_3D('',#11059,#9058,#9059) ;
#8299 = AXIS2_PLACEMENT_3D('',#11069,#9060,#9061) ;
#8300 = AXIS2_PLACEMENT_3D('',#11089,#9063,#9064) ;
#8301 = AXIS2_PLACEMENT_3D('',#11098,#9066,#9067) ;
#8302 = AXIS2_PLACEMENT_3D('',#11119,#9069,#9070) ;
#8303 = AXIS2_PLACEMENT_3D('',#11136,#9072,#9073) ;
#8304 = AXIS2_PLACEMENT_3D('',#11137,#9074,#9075) ;
#8305 = AXIS2_PLACEMENT_3D('',#11158,#9077,#9078) ;
#8306 = AXIS2_PLACEMENT_3D('',#11175,#9080,#9081) ;
#8307 = AXIS2_PLACEMENT_3D('',#11176,#9082,#9083) ;
#8308 = AXIS2_PLACEMENT_3D('',#11177,#9084,#9085) ;
#8309 = AXIS2_PLACEMENT_3D('',#11178,#9086,#9087) ;
#8310 = AXIS2_PLACEMENT_3D('',#11179,#9088,#9089) ;
#8311 = AXIS2_PLACEMENT_3D('',#11180,#9090,#9091) ;
#8312 = AXIS2_PLACEMENT_3D('',#11181,#9092,#9093) ;
#8313 = AXIS2_PLACEMENT_3D('',#11182,#9094,#9095) ;
#8314 = AXIS2_PLACEMENT_3D('',#11183,#9096,#9097) ;
#8315 = AXIS2_PLACEMENT_3D('',#11184,#9098,#9099) ;
#8316 = AXIS2_PLACEMENT_3D('',#11185,#9100,#9101) ;
#8317 = AXIS2_PLACEMENT_3D('',#11186,#9102,#9103) ;
#8318 = AXIS2_PLACEMENT_3D('',#11187,#9104,#9105) ;
#8319 = AXIS2_PLACEMENT_3D('',#11188,#9106,#9107) ;
#8320 = AXIS2_PLACEMENT_3D('',#11189,#9108,#9109) ;
#8321 = AXIS2_PLACEMENT_3D('',#11190,#9110,#9111) ;
#8322 = AXIS2_PLACEMENT_3D('',#11191,#9112,#9113) ;
#8323 = AXIS2_PLACEMENT_3D('',#11192,#9114,#9115) ;
#8324 = AXIS2_PLACEMENT_3D('',#11193,#9116,#9117) ;
#8325 = AXIS2_PLACEMENT_3D('',#11194,#9118,#9119) ;
#8326 = AXIS2_PLACEMENT_3D('',#11195,#9120,#9121) ;
#8327 = AXIS2_PLACEMENT_3D('',#11196,#9122,#9123) ;
#8328 = AXIS2_PLACEMENT_3D('',#11197,#9124,#9125) ;
#8329 = AXIS2_PLACEMENT_3D('',#11198,#9126,#9127) ;
#8330 = AXIS2_PLACEMENT_3D('',#11199,#9128,#9129) ;
#8331 = AXIS2_PLACEMENT_3D('',#11200,#9130,#9131) ;
#8332 = AXIS2_PLACEMENT_3D('',#11201,#9132,#9133) ;
#8333 = AXIS2_PLACEMENT_3D('',#11202,#9134,#9135) ;
#8334 = AXIS2_PLACEMENT_3D('',#11203,#9136,#9137) ;
#8335 = AXIS2_PLACEMENT_3D('',#11204,#9138,#9139) ;
#8336 = AXIS2_PLACEMENT_3D('',#11206,#9140,#9141) ;
#8337 = AXIS2_PLACEMENT_3D('',#11207,#9142,#9143) ;
#8338 = AXIS2_PLACEMENT_3D('',#11209,#9144,#9145) ;
#8339 = AXIS2_PLACEMENT_3D('',#11211,#9147,#9148) ;
#8340 = AXIS2_PLACEMENT_3D('',#11213,#9150,#9151) ;
#8341 = AXIS2_PLACEMENT_3D('',#11215,#9152,#9153) ;
#8342 = AXIS2_PLACEMENT_3D('',#11216,#9154,#9155) ;
#8343 = AXIS2_PLACEMENT_3D('',#11218,#9156,#9157) ;
#8344 = AXIS2_PLACEMENT_3D('',#11221,#9160,#9161) ;
#8345 = AXIS2_PLACEMENT_3D('',#11223,#9163,#9164) ;
#8346 = AXIS2_PLACEMENT_3D('',#11757,#9192,#9193) ;
#8347 = AXIS2_PLACEMENT_3D('',#11759,#9194,#9195) ;
#8348 = AXIS2_PLACEMENT_3D('',#11779,#9198,#9199) ;
#8349 = AXIS2_PLACEMENT_3D('',#11802,#9202,#9203) ;
#8350 = AXIS2_PLACEMENT_3D('',#11804,#9204,#9205) ;
#8351 = AXIS2_PLACEMENT_3D('',#11846,#9210,#9211) ;
#8352 = AXIS2_PLACEMENT_3D('',#11871,#9216,#9217) ;
#8353 = AXIS2_PLACEMENT_3D('',#11873,#9218,#9219) ;
#8354 = AXIS2_PLACEMENT_3D('',#11877,#9222,#9223) ;
#8355 = AXIS2_PLACEMENT_3D('',#11883,#9227,#9228) ;
#8356 = AXIS2_PLACEMENT_3D('',#11884,#9229,#9230) ;
#8357 = AXIS2_PLACEMENT_3D('',#11886,#9232,#9233) ;
#8358 = AXIS2_PLACEMENT_3D('',#11887,#9234,#9235) ;
#8359 = AXIS2_PLACEMENT_3D('',#11889,#9236,#9237) ;
#8360 = AXIS2_PLACEMENT_3D('',#11892,#9239,#9240) ;
#8361 = AXIS2_PLACEMENT_3D('',#11895,#9241,#9242) ;
#8362 = AXIS2_PLACEMENT_3D('',#11899,#9244,#9245) ;
#8363 = AXIS2_PLACEMENT_3D('',#11903,#9247,#9248) ;
#8364 = AXIS2_PLACEMENT_3D('',#11957,#9249,#9250) ;
#8365 = AXIS2_PLACEMENT_3D('',#11961,#9252,#9253) ;
#8366 = AXIS2_PLACEMENT_3D('',#11965,#9255,#9256) ;
#8367 = AXIS2_PLACEMENT_3D('',#11967,#9257,#9258) ;
#8368 = AXIS2_PLACEMENT_3D('',#11970,#9260,#9261) ;
#8369 = AXIS2_PLACEMENT_3D('',#11989,#9262,#9263) ;
#8370 = AXIS2_PLACEMENT_3D('',#12156,#9264,#9265) ;
#8371 = AXIS2_PLACEMENT_3D('',#12318,#9266,#9267) ;
#8372 = AXIS2_PLACEMENT_3D('',#12322,#9269,#9270) ;
#8373 = AXIS2_PLACEMENT_3D('',#12387,#9271,#9272) ;
#8374 = AXIS2_PLACEMENT_3D('',#12391,#9274,#9275) ;
#8375 = AXIS2_PLACEMENT_3D('',#12440,#9276,#9277) ;
#8376 = AXIS2_PLACEMENT_3D('',#12444,#9279,#9280) ;
#8377 = AXIS2_PLACEMENT_3D('',#12448,#9282,#9283) ;
#8378 = AXIS2_PLACEMENT_3D('',#12502,#9284,#9285) ;
#8379 = AXIS2_PLACEMENT_3D('',#12506,#9287,#9288) ;
#8380 = AXIS2_PLACEMENT_3D('',#12510,#9290,#9291) ;
#8381 = AXIS2_PLACEMENT_3D('',#12512,#9292,#9293) ;
#8382 = AXIS2_PLACEMENT_3D('',#12515,#9295,#9296) ;
#8383 = AXIS2_PLACEMENT_3D('',#12518,#9297,#9298) ;
#8384 = AXIS2_PLACEMENT_3D('',#12522,#9300,#9301) ;
#8385 = AXIS2_PLACEMENT_3D('',#12526,#9303,#9304) ;
#8386 = AXIS2_PLACEMENT_3D('',#12530,#9306,#9307) ;
#8387 = AXIS2_PLACEMENT_3D('',#12532,#9309,#9310) ;
#8388 = AXIS2_PLACEMENT_3D('',#12538,#9314,#9315) ;
#8389 = AXIS2_PLACEMENT_3D('',#12542,#9318,#9319) ;
#8390 = AXIS2_PLACEMENT_3D('',#12546,#9322,#9323) ;
#8391 = AXIS2_PLACEMENT_3D('',#12548,#9325,#9326) ;
#8392 = AXIS2_PLACEMENT_3D('',#12549,#9327,#9328) ;
#8393 = AXIS2_PLACEMENT_3D('',#12555,#9332,#9333) ;
#8394 = AXIS2_PLACEMENT_3D('',#12559,#9336,#9337) ;
#8395 = AXIS2_PLACEMENT_3D('',#12563,#9340,#9341) ;
#8396 = AXIS2_PLACEMENT_3D('',#12565,#9343,#9344) ;
#8397 = AXIS2_PLACEMENT_3D('',#12566,#9345,#9346) ;
#8398 = AXIS2_PLACEMENT_3D('',#12572,#9350,#9351) ;
#8399 = AXIS2_PLACEMENT_3D('',#12576,#9354,#9355) ;
#8400 = AXIS2_PLACEMENT_3D('',#12580,#9358,#9359) ;
#8401 = AXIS2_PLACEMENT_3D('',#12584,#9362,#9363) ;
#8402 = AXIS2_PLACEMENT_3D('',#12588,#9366,#9367) ;
#8403 = AXIS2_PLACEMENT_3D('',#12592,#9370,#9371) ;
#8404 = AXIS2_PLACEMENT_3D('',#12596,#9374,#9375) ;
#8405 = AXIS2_PLACEMENT_3D('',#12600,#9378,#9379) ;
#8406 = AXIS2_PLACEMENT_3D('',#12626,#9384,#9385) ;
#8407 = AXIS2_PLACEMENT_3D('',#12630,#9388,#9389) ;
#8408 = AXIS2_PLACEMENT_3D('',#12634,#9392,#9393) ;
#8409 = AXIS2_PLACEMENT_3D('',#12638,#9396,#9397) ;
#8410 = AXIS2_PLACEMENT_3D('',#12640,#9399,#9400) ;
#8411 = AXIS2_PLACEMENT_3D('',#12654,#9403,#9404) ;
#8412 = AXIS2_PLACEMENT_3D('',#12658,#9407,#9408) ;
#8413 = AXIS2_PLACEMENT_3D('',#12662,#9411,#9412) ;
#8414 = AXIS2_PLACEMENT_3D('',#12776,#9425,#9426) ;
#8415 = AXIS2_PLACEMENT_3D('',#12780,#9429,#9430) ;
#8416 = AXIS2_PLACEMENT_3D('',#12784,#9433,#9434) ;
#8417 = AXIS2_PLACEMENT_3D('',#12786,#9436,#9437) ;
#8418 = AXIS2_PLACEMENT_3D('',#12822,#9442,#9443) ;
#8419 = AXIS2_PLACEMENT_3D('',#13145,#9475,#9476) ;
#8420 = AXIS2_PLACEMENT_3D('',#13158,#9479,#9480) ;
#8421 = AXIS2_PLACEMENT_3D('',#13159,#9481,#9482) ;
#8422 = AXIS2_PLACEMENT_3D('',#13165,#9486,#9487) ;
#8423 = AXIS2_PLACEMENT_3D('',#13169,#9490,#9491) ;
#8424 = AXIS2_PLACEMENT_3D('',#13173,#9494,#9495) ;
#8425 = AXIS2_PLACEMENT_3D('',#13177,#9498,#9499) ;
#8426 = AXIS2_PLACEMENT_3D('',#13181,#9502,#9503) ;
#8427 = AXIS2_PLACEMENT_3D('',#13185,#9506,#9507) ;
#8428 = AXIS2_PLACEMENT_3D('',#13189,#9510,#9511) ;
#8429 = AXIS2_PLACEMENT_3D('',#13193,#9514,#9515) ;
#8430 = AXIS2_PLACEMENT_3D('',#13219,#9520,#9521) ;
#8431 = AXIS2_PLACEMENT_3D('',#13223,#9524,#9525) ;
#8432 = AXIS2_PLACEMENT_3D('',#13227,#9528,#9529) ;
#8433 = AXIS2_PLACEMENT_3D('',#13231,#9532,#9533) ;
#8434 = AXIS2_PLACEMENT_3D('',#13233,#9535,#9536) ;
#8435 = AXIS2_PLACEMENT_3D('',#13234,#9537,#9538) ;
#8436 = AXIS2_PLACEMENT_3D('',#13236,#9539,#9540) ;
#8437 = AXIS2_PLACEMENT_3D('',#13239,#9542,#9543) ;
#8438 = AXIS2_PLACEMENT_3D('',#13240,#9544,#9545) ;
#8439 = AXIS2_PLACEMENT_3D('',#13242,#9546,#9547) ;
#8440 = AXIS2_PLACEMENT_3D('',#13243,#9548,#9549) ;
#8441 = AXIS2_PLACEMENT_3D('',#13244,#9550,#9551) ;
#8442 = AXIS2_PLACEMENT_3D('',#13245,#9552,#9553) ;
#8443 = AXIS2_PLACEMENT_3D('',#13250,#9555,#9556) ;
#8444 = AXIS2_PLACEMENT_3D('',#13252,#9557,#9558) ;
#8445 = AXIS2_PLACEMENT_3D('',#13255,#9560,#9561) ;
#8446 = AXIS2_PLACEMENT_3D('',#13292,#9562,#9563) ;
#8447 = AXIS2_PLACEMENT_3D('',#13294,#9564,#9565) ;
#8448 = AXIS2_PLACEMENT_3D('',#13303,#9566,#9567) ;
#8449 = AXIS2_PLACEMENT_3D('',#13312,#9568,#9569) ;
#8450 = AXIS2_PLACEMENT_3D('',#13321,#9570,#9571) ;
#8451 = AXIS2_PLACEMENT_3D('',#13323,#9572,#9573) ;
#8452 = AXIS2_PLACEMENT_3D('',#13325,#9574,#9575) ;
#8453 = AXIS2_PLACEMENT_3D('',#13326,#9576,#9577) ;
#8454 = AXIS2_PLACEMENT_3D('',#13327,#9578,#9579) ;
#8455 = AXIS2_PLACEMENT_3D('',#13328,#9580,#9581) ;
#8456 = AXIS2_PLACEMENT_3D('',#13331,#9583,#9584) ;
#8457 = AXIS2_PLACEMENT_3D('',#13332,#9585,#9586) ;
#8458 = AXIS2_PLACEMENT_3D('',#13336,#9588,#9589) ;
#8459 = AXIS2_PLACEMENT_3D('',#13338,#9590,#9591) ;
#8460 = AXIS2_PLACEMENT_3D('',#13340,#9593,#9594) ;
#8461 = AXIS2_PLACEMENT_3D('',#13371,#9595,#9596) ;
#8462 = AXIS2_PLACEMENT_3D('',#13374,#9598,#9599) ;
#8463 = AXIS2_PLACEMENT_3D('',#13375,#9600,#9601) ;
#8464 = AXIS2_PLACEMENT_3D('',#13379,#9603,#9604) ;
#8465 = AXIS2_PLACEMENT_3D('',#13381,#9605,#9606) ;
#8466 = AXIS2_PLACEMENT_3D('',#13383,#9608,#9609) ;
#8467 = AXIS2_PLACEMENT_3D('',#13414,#9610,#9611) ;
#8468 = AXIS2_PLACEMENT_3D('',#13417,#9613,#9614) ;
#8469 = AXIS2_PLACEMENT_3D('',#13418,#9615,#9616) ;
#8470 = AXIS2_PLACEMENT_3D('',#13422,#9618,#9619) ;
#8471 = AXIS2_PLACEMENT_3D('',#13424,#9620,#9621) ;
#8472 = AXIS2_PLACEMENT_3D('',#13426,#9623,#9624) ;
#8473 = AXIS2_PLACEMENT_3D('',#13457,#9625,#9626) ;
#8474 = AXIS2_PLACEMENT_3D('',#13460,#9628,#9629) ;
#8475 = AXIS2_PLACEMENT_3D('',#13461,#9630,#9631) ;
#8476 = AXIS2_PLACEMENT_3D('',#13463,#9632,#9633) ;
#8477 = AXIS2_PLACEMENT_3D('',#13464,#9634,#9635) ;
#8478 = AXIS2_PLACEMENT_3D('',#13466,#9636,#9637) ;
#8479 = AXIS2_PLACEMENT_3D('',#13467,#9638,#9639) ;
#8480 = AXIS2_PLACEMENT_3D('',#13469,#9640,#9641) ;
#8481 = AXIS2_PLACEMENT_3D('',#13470,#9642,#9643) ;
#8482 = AXIS2_PLACEMENT_3D('',#13472,#9644,#9645) ;
#8483 = AXIS2_PLACEMENT_3D('',#13473,#9646,#9647) ;
#8484 = AXIS2_PLACEMENT_3D('',#13476,#9649,#9650) ;
#8485 = AXIS2_PLACEMENT_3D('',#13477,#9651,#9652) ;
#8486 = AXIS2_PLACEMENT_3D('',#13480,#9654,#9655) ;
#8487 = AXIS2_PLACEMENT_3D('',#13481,#9656,#9657) ;
#8488 = AXIS2_PLACEMENT_3D('',#13484,#9659,#9660) ;
#8489 = AXIS2_PLACEMENT_3D('',#13485,#9661,#9662) ;
#8490 = AXIS2_PLACEMENT_3D('',#13488,#9664,#9665) ;
#8491 = AXIS2_PLACEMENT_3D('',#13489,#9666,#9667) ;
#8492 = AXIS2_PLACEMENT_3D('',#13494,#9669,#9670) ;
#8493 = AXIS2_PLACEMENT_3D('',#13497,#9672,#9673) ;
#8494 = AXIS2_PLACEMENT_3D('',#13498,#9674,#9675) ;
#8495 = AXIS2_PLACEMENT_3D('',#13503,#9677,#9678) ;
#8496 = AXIS2_PLACEMENT_3D('',#13506,#9680,#9681) ;
#8497 = AXIS2_PLACEMENT_3D('',#13507,#9682,#9683) ;
#8498 = AXIS2_PLACEMENT_3D('',#13512,#9685,#9686) ;
#8499 = AXIS2_PLACEMENT_3D('',#13515,#9688,#9689) ;
#8500 = AXIS2_PLACEMENT_3D('',#13516,#9690,#9691) ;
#8501 = AXIS2_PLACEMENT_3D('',#13521,#9693,#9694) ;
#8502 = AXIS2_PLACEMENT_3D('',#13524,#9696,#9697) ;
#8503 = AXIS2_PLACEMENT_3D('',#13525,#9698,#9699) ;
#8504 = AXIS2_PLACEMENT_3D('',#13527,#9700,#9701) ;
#8505 = AXIS2_PLACEMENT_3D('',#13528,#9702,#9703) ;
#8506 = AXIS2_PLACEMENT_3D('',#13529,#9704,#9705) ;
#8507 = AXIS2_PLACEMENT_3D('',#13530,#9706,#9707) ;
#8508 = AXIS2_PLACEMENT_3D('',#13531,#9708,#9709) ;
#8509 = AXIS2_PLACEMENT_3D('',#13532,#9710,#9711) ;
#8510 = AXIS2_PLACEMENT_3D('',#13533,#9712,#9713) ;
#8511 = AXIS2_PLACEMENT_3D('',#13534,#9714,#9715) ;
#8512 = AXIS2_PLACEMENT_3D('',#13535,#9716,#9717) ;
#8513 = AXIS2_PLACEMENT_3D('',#13536,#9718,#9719) ;
#8514 = AXIS2_PLACEMENT_3D('',#13537,#9720,#9721) ;
#8515 = AXIS2_PLACEMENT_3D('',#13538,#9722,#9723) ;
#8516 = AXIS2_PLACEMENT_3D('',#13539,#9724,#9725) ;
#8517 = AXIS2_PLACEMENT_3D('',#13540,#9726,#9727) ;
#8518 = AXIS2_PLACEMENT_3D('',#13542,#9728,#9729) ;
#8519 = AXIS2_PLACEMENT_3D('',#13543,#9730,#9731) ;
#8520 = AXIS2_PLACEMENT_3D('',#13545,#9733,#9734) ;
#8521 = AXIS2_PLACEMENT_3D('',#13547,#9735,#9736) ;
#8522 = AXIS2_PLACEMENT_3D('',#13549,#9737,#9738) ;
#8523 = AXIS2_PLACEMENT_3D('',#13550,#9739,#9740) ;
#8524 = AXIS2_PLACEMENT_3D('',#13553,#9742,#9743) ;
#8525 = AXIS2_PLACEMENT_3D('',#13554,#9744,#9745) ;
#8526 = AXIS2_PLACEMENT_3D('',#13556,#9746,#9747) ;
#8527 = AXIS2_PLACEMENT_3D('',#13557,#9748,#9749) ;
#8528 = AXIS2_PLACEMENT_3D('',#13559,#9750,#9751) ;
#8529 = AXIS2_PLACEMENT_3D('',#13561,#9753,#9754) ;
#8530 = AXIS2_PLACEMENT_3D('',#13563,#9755,#9756) ;
#8531 = AXIS2_PLACEMENT_3D('',#13565,#9757,#9758) ;
#8532 = AXIS2_PLACEMENT_3D('',#13566,#9759,#9760) ;
#8533 = AXIS2_PLACEMENT_3D('',#13569,#9762,#9763) ;
#8534 = AXIS2_PLACEMENT_3D('',#13570,#9764,#9765) ;
#8535 = AXIS2_PLACEMENT_3D('',#13572,#9766,#9767) ;
#8536 = AXIS2_PLACEMENT_3D('',#13573,#9768,#9769) ;
#8537 = AXIS2_PLACEMENT_3D('',#13575,#9770,#9771) ;
#8538 = AXIS2_PLACEMENT_3D('',#13577,#9773,#9774) ;
#8539 = AXIS2_PLACEMENT_3D('',#13578,#9775,#9776) ;
#8540 = AXIS2_PLACEMENT_3D('',#13581,#9778,#9779) ;
#8541 = AXIS2_PLACEMENT_3D('',#13582,#9780,#9781) ;
#8542 = AXIS2_PLACEMENT_3D('',#13584,#9782,#9783) ;
#8543 = AXIS2_PLACEMENT_3D('',#13585,#9784,#9785) ;
#8544 = AXIS2_PLACEMENT_3D('',#13587,#9786,#9787) ;
#8545 = AXIS2_PLACEMENT_3D('',#13589,#9789,#9790) ;
#8546 = AXIS2_PLACEMENT_3D('',#13591,#9791,#9792) ;
#8547 = AXIS2_PLACEMENT_3D('',#13593,#9794,#9795) ;
#8548 = AXIS2_PLACEMENT_3D('',#13595,#9797,#9798) ;
#8549 = AXIS2_PLACEMENT_3D('',#13597,#9799,#9800) ;
#8550 = AXIS2_PLACEMENT_3D('',#13599,#9802,#9803) ;
#8551 = AXIS2_PLACEMENT_3D('',#13600,#9804,#9805) ;
#8552 = AXIS2_PLACEMENT_3D('',#13602,#9807,#9808) ;
#8553 = AXIS2_PLACEMENT_3D('',#13603,#9809,#9810) ;
#8554 = AXIS2_PLACEMENT_3D('',#13612,#9815,#9816) ;
#8555 = AXIS2_PLACEMENT_3D('',#13614,#9817,#9818) ;
#8556 = AXIS2_PLACEMENT_3D('',#13616,#9819,#9820) ;
#8557 = AXIS2_PLACEMENT_3D('',#13618,#9822,#9823) ;
#8558 = AXIS2_PLACEMENT_3D('',#13624,#9827,#9828) ;
#8559 = AXIS2_PLACEMENT_3D('',#13625,#9829,#9830) ;
#8560 = AXIS2_PLACEMENT_3D('',#13626,#9831,#9832) ;
#8561 = AXIS2_PLACEMENT_3D('',#13627,#9833,#9834) ;
#8562 = AXIS2_PLACEMENT_3D('',#13636,#9839,#9840) ;
#8563 = AXIS2_PLACEMENT_3D('',#13638,#9841,#9842) ;
#8564 = AXIS2_PLACEMENT_3D('',#13640,#9843,#9844) ;
#8565 = AXIS2_PLACEMENT_3D('',#13642,#9846,#9847) ;
#8566 = AXIS2_PLACEMENT_3D('',#13648,#9851,#9852) ;
#8567 = AXIS2_PLACEMENT_3D('',#13649,#9853,#9854) ;
#8568 = AXIS2_PLACEMENT_3D('',#13650,#9855,#9856) ;
#8569 = AXIS2_PLACEMENT_3D('',#13651,#9857,#9858) ;
#8570 = AXIS2_PLACEMENT_3D('',#13660,#9863,#9864) ;
#8571 = AXIS2_PLACEMENT_3D('',#13662,#9865,#9866) ;
#8572 = AXIS2_PLACEMENT_3D('',#13664,#9867,#9868) ;
#8573 = AXIS2_PLACEMENT_3D('',#13666,#9870,#9871) ;
#8574 = AXIS2_PLACEMENT_3D('',#13672,#9875,#9876) ;
#8575 = AXIS2_PLACEMENT_3D('',#13673,#9877,#9878) ;
#8576 = AXIS2_PLACEMENT_3D('',#13674,#9879,#9880) ;
#8577 = AXIS2_PLACEMENT_3D('',#13675,#9881,#9882) ;
#8578 = AXIS2_PLACEMENT_3D('',#13684,#9887,#9888) ;
#8579 = AXIS2_PLACEMENT_3D('',#13686,#9889,#9890) ;
#8580 = AXIS2_PLACEMENT_3D('',#13688,#9891,#9892) ;
#8581 = AXIS2_PLACEMENT_3D('',#13690,#9894,#9895) ;
#8582 = AXIS2_PLACEMENT_3D('',#13696,#9899,#9900) ;
#8583 = AXIS2_PLACEMENT_3D('',#13697,#9901,#9902) ;
#8584 = AXIS2_PLACEMENT_3D('',#13698,#9903,#9904) ;
#8585 = AXIS2_PLACEMENT_3D('',#13699,#9905,#9906) ;
#8586 = AXIS2_PLACEMENT_3D('',#13701,#9907,#9908) ;
#8587 = AXIS2_PLACEMENT_3D('',#13704,#9910,#9911) ;
#8588 = AXIS2_PLACEMENT_3D('',#13705,#9912,#9913) ;
#8589 = AXIS2_PLACEMENT_3D('',#13707,#9914,#9915) ;
#8590 = AXIS2_PLACEMENT_3D('',#13708,#9916,#9917) ;
#8591 = AXIS2_PLACEMENT_3D('',#13710,#9918,#9919) ;
#8592 = AXIS2_PLACEMENT_3D('',#13712,#9921,#9922) ;
#8593 = AXIS2_PLACEMENT_3D('',#13713,#9923,#9924) ;
#8594 = AXIS2_PLACEMENT_3D('',#13714,#9925,#9926) ;
#8595 = AXIS2_PLACEMENT_3D('',#13717,#9927,#9928) ;
#8596 = AXIS2_PLACEMENT_3D('',#13718,#9929,#9930) ;
#8597 = AXIS2_PLACEMENT_3D('',#13719,#9931,#9932) ;
#8598 = AXIS2_PLACEMENT_3D('',#13735,#9934,#9935) ;
#8599 = AXIS2_PLACEMENT_3D('',#13743,#9936,#9937) ;
#8600 = AXIS2_PLACEMENT_3D('',#13791,#9939,#9940) ;
#8601 = AXIS2_PLACEMENT_3D('',#13839,#9942,#9943) ;
#8602 = AXIS2_PLACEMENT_3D('',#13893,#9945,#9946) ;
#8603 = AXIS2_PLACEMENT_3D('',#13941,#9948,#9949) ;
#8604 = AXIS2_PLACEMENT_3D('',#13989,#9951,#9952) ;
#8605 = AXIS2_PLACEMENT_3D('',#14043,#9954,#9955) ;
#8606 = AXIS2_PLACEMENT_3D('',#14091,#9957,#9958) ;
#8607 = AXIS2_PLACEMENT_3D('',#14139,#9960,#9961) ;
#8608 = AXIS2_PLACEMENT_3D('',#14187,#9963,#9964) ;
#8609 = AXIS2_PLACEMENT_3D('',#14241,#9966,#9967) ;
#8610 = AXIS2_PLACEMENT_3D('',#14289,#9969,#9970) ;
#8611 = AXIS2_PLACEMENT_3D('',#14337,#9972,#9973) ;
#8612 = AXIS2_PLACEMENT_3D('',#14342,#9975,#9976) ;
#8613 = AXIS2_PLACEMENT_3D('',#14390,#9977,#9978) ;
#8614 = AXIS2_PLACEMENT_3D('',#14404,#9980,#9981) ;
#8615 = AXIS2_PLACEMENT_3D('',#14411,#9982,#9983) ;
#8616 = AXIS2_PLACEMENT_3D('',#14436,#9985,#9986) ;
#8617 = AXIS2_PLACEMENT_3D('',#14460,#9988,#9989) ;
#8618 = AXIS2_PLACEMENT_3D('',#14485,#9991,#9992) ;
#8619 = AXIS2_PLACEMENT_3D('',#14510,#9994,#9995) ;
#8620 = AXIS2_PLACEMENT_3D('',#14534,#9997,#9998) ;
#8621 = AXIS2_PLACEMENT_3D('',#14558,#10000,#10001) ;
#8622 = AXIS2_PLACEMENT_3D('',#14583,#10003,#10004) ;
#8623 = AXIS2_PLACEMENT_3D('',#14608,#10006,#10007) ;
#8624 = AXIS2_PLACEMENT_3D('',#14632,#10009,#10010) ;
#8625 = AXIS2_PLACEMENT_3D('',#14657,#10012,#10013) ;
#8626 = AXIS2_PLACEMENT_3D('',#14682,#10015,#10016) ;
#8627 = AXIS2_PLACEMENT_3D('',#14706,#10018,#10019) ;
#8628 = AXIS2_PLACEMENT_3D('',#14796,#10020,#10021) ;
#8629 = AXIS2_PLACEMENT_3D('',#15343,#10022,#10023) ;
#8630 = AXIS2_PLACEMENT_3D('',#15345,#10024,#10025) ;
#8631 = AXIS2_PLACEMENT_3D('',#15435,#10026,#10027) ;
#8632 = AXIS2_PLACEMENT_3D('',#15436,#10028,#10029) ;
#8633 = AXIS2_PLACEMENT_3D('',#15437,#10030,#10031) ;
#8634 = AXIS2_PLACEMENT_3D('',#15802,#10032,#10033) ;
#8635 = AXIS2_PLACEMENT_3D('',#15804,#10034,#10035) ;
#8636 = AXIS2_PLACEMENT_3D('',#15805,#10036,#10037) ;
#8637 = AXIS2_PLACEMENT_3D('',#15806,#10038,#10039) ;
#8638 = AXIS2_PLACEMENT_3D('',#15807,#10040,#10041) ;
#8639 = AXIS2_PLACEMENT_3D('',#15808,#10042,#10043) ;
#8640 = AXIS2_PLACEMENT_3D('',#15810,#10044,#10045) ;
#8641 = AXIS2_PLACEMENT_3D('',#15811,#10046,#10047) ;
#8642 = AXIS2_PLACEMENT_3D('',#15814,#10049,#10050) ;
#8643 = AXIS2_PLACEMENT_3D('',#15815,#10051,#10052) ;
#8644 = AXIS2_PLACEMENT_3D('',#15816,#10053,#10054) ;
#8645 = AXIS2_PLACEMENT_3D('',#15827,#10058,#10059) ;
#8646 = AXIS2_PLACEMENT_3D('',#15829,#10060,#10061) ;
#8647 = AXIS2_PLACEMENT_3D('',#15831,#10063,#10064) ;
#8648 = AXIS2_PLACEMENT_3D('',#15837,#10066,#10067) ;
#8649 = AXIS2_PLACEMENT_3D('',#15839,#10068,#10069) ;
#8650 = AXIS2_PLACEMENT_3D('',#15843,#10071,#10072) ;
#8651 = AXIS2_PLACEMENT_3D('',#15847,#10074,#10075) ;
#8652 = AXIS2_PLACEMENT_3D('',#15851,#10077,#10078) ;
#8653 = AXIS2_PLACEMENT_3D('',#15855,#10080,#10081) ;
#8654 = AXIS2_PLACEMENT_3D('',#15859,#10083,#10084) ;
#8655 = AXIS2_PLACEMENT_3D('',#15863,#10086,#10087) ;
#8656 = AXIS2_PLACEMENT_3D('',#15867,#10089,#10090) ;
#8657 = AXIS2_PLACEMENT_3D('',#15871,#10092,#10093) ;
#8658 = AXIS2_PLACEMENT_3D('',#15875,#10095,#10096) ;
#8659 = AXIS2_PLACEMENT_3D('',#15879,#10098,#10099) ;
#8660 = AXIS2_PLACEMENT_3D('',#15883,#10101,#10102) ;
#8661 = AXIS2_PLACEMENT_3D('',#15887,#10104,#10105) ;
#8662 = AXIS2_PLACEMENT_3D('',#15891,#10107,#10108) ;
#8663 = AXIS2_PLACEMENT_3D('',#15895,#10110,#10111) ;
#8664 = AXIS2_PLACEMENT_3D('',#15899,#10113,#10114) ;
#8665 = AXIS2_PLACEMENT_3D('',#15903,#10116,#10117) ;
#8666 = AXIS2_PLACEMENT_3D('',#15907,#10119,#10120) ;
#8667 = AXIS2_PLACEMENT_3D('',#15911,#10122,#10123) ;
#8668 = AXIS2_PLACEMENT_3D('',#15915,#10125,#10126) ;
#8669 = AXIS2_PLACEMENT_3D('',#15919,#10128,#10129) ;
#8670 = AXIS2_PLACEMENT_3D('',#15923,#10131,#10132) ;
#8671 = AXIS2_PLACEMENT_3D('',#15927,#10134,#10135) ;
#8672 = AXIS2_PLACEMENT_3D('',#15931,#10137,#10138) ;
#8673 = AXIS2_PLACEMENT_3D('',#15935,#10140,#10141) ;
#8674 = AXIS2_PLACEMENT_3D('',#15939,#10143,#10144) ;
#8675 = AXIS2_PLACEMENT_3D('',#15943,#10146,#10147) ;
#8676 = AXIS2_PLACEMENT_3D('',#15947,#10149,#10150) ;
#8677 = AXIS2_PLACEMENT_3D('',#15951,#10152,#10153) ;
#8678 = AXIS2_PLACEMENT_3D('',#15955,#10155,#10156) ;
#8679 = AXIS2_PLACEMENT_3D('',#15959,#10158,#10159) ;
#8680 = AXIS2_PLACEMENT_3D('',#15963,#10161,#10162) ;
#8681 = AXIS2_PLACEMENT_3D('',#15967,#10164,#10165) ;
#8682 = AXIS2_PLACEMENT_3D('',#15971,#10167,#10168) ;
#8683 = AXIS2_PLACEMENT_3D('',#15975,#10170,#10171) ;
#8684 = AXIS2_PLACEMENT_3D('',#15979,#10173,#10174) ;
#8685 = AXIS2_PLACEMENT_3D('',#15983,#10176,#10177) ;
#8686 = AXIS2_PLACEMENT_3D('',#15987,#10179,#10180) ;
#8687 = AXIS2_PLACEMENT_3D('',#15991,#10182,#10183) ;
#8688 = AXIS2_PLACEMENT_3D('',#15995,#10185,#10186) ;
#8689 = AXIS2_PLACEMENT_3D('',#15999,#10188,#10189) ;
#8690 = AXIS2_PLACEMENT_3D('',#16003,#10191,#10192) ;
#8691 = AXIS2_PLACEMENT_3D('',#16007,#10194,#10195) ;
#8692 = AXIS2_PLACEMENT_3D('',#16011,#10197,#10198) ;
#8693 = AXIS2_PLACEMENT_3D('',#16015,#10200,#10201) ;
#8694 = AXIS2_PLACEMENT_3D('',#16019,#10203,#10204) ;
#8695 = AXIS2_PLACEMENT_3D('',#16023,#10206,#10207) ;
#8696 = AXIS2_PLACEMENT_3D('',#16027,#10209,#10210) ;
#8697 = AXIS2_PLACEMENT_3D('',#16031,#10212,#10213) ;
#8698 = AXIS2_PLACEMENT_3D('',#16035,#10215,#10216) ;
#8699 = AXIS2_PLACEMENT_3D('',#16039,#10218,#10219) ;
#8700 = AXIS2_PLACEMENT_3D('',#16043,#10221,#10222) ;
#8701 = AXIS2_PLACEMENT_3D('',#16047,#10224,#10225) ;
#8702 = AXIS2_PLACEMENT_3D('',#16051,#10227,#10228) ;
#8703 = AXIS2_PLACEMENT_3D('',#16055,#10230,#10231) ;
#8704 = AXIS2_PLACEMENT_3D('',#16059,#10233,#10234) ;
#8705 = AXIS2_PLACEMENT_3D('',#16062,#10236,#10237) ;
#8706 = AXIS2_PLACEMENT_3D('',#16064,#10238,#10239) ;
#8707 = AXIS2_PLACEMENT_3D('',#16068,#10241,#10242) ;
#8708 = AXIS2_PLACEMENT_3D('',#16072,#10244,#10245) ;
#8709 = AXIS2_PLACEMENT_3D('',#16076,#10247,#10248) ;
#8710 = AXIS2_PLACEMENT_3D('',#16080,#10250,#10251) ;
#8711 = AXIS2_PLACEMENT_3D('',#16084,#10253,#10254) ;
#8712 = AXIS2_PLACEMENT_3D('',#16088,#10256,#10257) ;
#8713 = AXIS2_PLACEMENT_3D('',#16092,#10259,#10260) ;
#8714 = AXIS2_PLACEMENT_3D('',#16096,#10262,#10263) ;
#8715 = AXIS2_PLACEMENT_3D('',#16100,#10265,#10266) ;
#8716 = AXIS2_PLACEMENT_3D('',#16104,#10268,#10269) ;
#8717 = AXIS2_PLACEMENT_3D('',#16108,#10271,#10272) ;
#8718 = AXIS2_PLACEMENT_3D('',#16112,#10274,#10275) ;
#8719 = AXIS2_PLACEMENT_3D('',#16116,#10277,#10278) ;
#8720 = AXIS2_PLACEMENT_3D('',#16120,#10280,#10281) ;
#8721 = AXIS2_PLACEMENT_3D('',#16123,#10283,#10284) ;
#8722 = AXIS2_PLACEMENT_3D('',#16124,#10285,#10286) ;
#8723 = AXIS2_PLACEMENT_3D('',#16132,#10289,#10290) ;
#8724 = AXIS2_PLACEMENT_3D('',#16134,#10292,#10293) ;
#8725 = AXIS2_PLACEMENT_3D('',#16138,#10294,#10295) ;
#8726 = AXIS2_PLACEMENT_3D('',#16146,#10298,#10299) ;
#8727 = AXIS2_PLACEMENT_3D('',#16148,#10301,#10302) ;
#8728 = AXIS2_PLACEMENT_3D('',#16152,#10303,#10304) ;
#8729 = AXIS2_PLACEMENT_3D('',#16160,#10307,#10308) ;
#8730 = AXIS2_PLACEMENT_3D('',#16162,#10310,#10311) ;
#8731 = AXIS2_PLACEMENT_3D('',#16166,#10312,#10313) ;
#8732 = AXIS2_PLACEMENT_3D('',#16174,#10316,#10317) ;
#8733 = AXIS2_PLACEMENT_3D('',#16176,#10319,#10320) ;
#8734 = AXIS2_PLACEMENT_3D('',#16180,#10321,#10322) ;
#8735 = AXIS2_PLACEMENT_3D('',#16188,#10325,#10326) ;
#8736 = AXIS2_PLACEMENT_3D('',#16190,#10328,#10329) ;
#8737 = AXIS2_PLACEMENT_3D('',#16194,#10330,#10331) ;
#8738 = AXIS2_PLACEMENT_3D('',#16202,#10334,#10335) ;
#8739 = AXIS2_PLACEMENT_3D('',#16204,#10337,#10338) ;
#8740 = AXIS2_PLACEMENT_3D('',#16208,#10339,#10340) ;
#8741 = AXIS2_PLACEMENT_3D('',#16216,#10343,#10344) ;
#8742 = AXIS2_PLACEMENT_3D('',#16218,#10346,#10347) ;
#8743 = AXIS2_PLACEMENT_3D('',#16222,#10348,#10349) ;
#8744 = AXIS2_PLACEMENT_3D('',#16230,#10352,#10353) ;
#8745 = AXIS2_PLACEMENT_3D('',#16232,#10355,#10356) ;
#8746 = AXIS2_PLACEMENT_3D('',#16236,#10357,#10358) ;
#8747 = AXIS2_PLACEMENT_3D('',#16244,#10361,#10362) ;
#8748 = AXIS2_PLACEMENT_3D('',#16246,#10364,#10365) ;
#8749 = AXIS2_PLACEMENT_3D('',#16250,#10366,#10367) ;
#8750 = AXIS2_PLACEMENT_3D('',#16258,#10370,#10371) ;
#8751 = AXIS2_PLACEMENT_3D('',#16260,#10373,#10374) ;
#8752 = AXIS2_PLACEMENT_3D('',#16264,#10375,#10376) ;
#8753 = AXIS2_PLACEMENT_3D('',#16272,#10379,#10380) ;
#8754 = AXIS2_PLACEMENT_3D('',#16274,#10382,#10383) ;
#8755 = AXIS2_PLACEMENT_3D('',#16278,#10384,#10385) ;
#8756 = AXIS2_PLACEMENT_3D('',#16286,#10388,#10389) ;
#8757 = AXIS2_PLACEMENT_3D('',#16288,#10391,#10392) ;
#8758 = AXIS2_PLACEMENT_3D('',#16292,#10393,#10394) ;
#8759 = AXIS2_PLACEMENT_3D('',#16300,#10397,#10398) ;
#8760 = AXIS2_PLACEMENT_3D('',#16302,#10400,#10401) ;
#8761 = AXIS2_PLACEMENT_3D('',#16306,#10402,#10403) ;
#8762 = AXIS2_PLACEMENT_3D('',#16314,#10406,#10407) ;
#8763 = AXIS2_PLACEMENT_3D('',#16316,#10409,#10410) ;
#8764 = AXIS2_PLACEMENT_3D('',#16320,#10411,#10412) ;
#8765 = AXIS2_PLACEMENT_3D('',#16328,#10415,#10416) ;
#8766 = AXIS2_PLACEMENT_3D('',#16330,#10418,#10419) ;
#8767 = AXIS2_PLACEMENT_3D('',#16334,#10420,#10421) ;
#8768 = AXIS2_PLACEMENT_3D('',#16342,#10424,#10425) ;
#8769 = AXIS2_PLACEMENT_3D('',#16344,#10427,#10428) ;
#8770 = AXIS2_PLACEMENT_3D('',#16348,#10429,#10430) ;
#8771 = AXIS2_PLACEMENT_3D('',#16356,#10433,#10434) ;
#8772 = AXIS2_PLACEMENT_3D('',#16358,#10436,#10437) ;
#8773 = AXIS2_PLACEMENT_3D('',#16362,#10438,#10439) ;
#8774 = AXIS2_PLACEMENT_3D('',#16370,#10442,#10443) ;
#8775 = AXIS2_PLACEMENT_3D('',#16372,#10445,#10446) ;
#8776 = AXIS2_PLACEMENT_3D('',#16376,#10447,#10448) ;
#8777 = AXIS2_PLACEMENT_3D('',#16384,#10451,#10452) ;
#8778 = AXIS2_PLACEMENT_3D('',#16386,#10454,#10455) ;
#8779 = AXIS2_PLACEMENT_3D('',#16390,#10456,#10457) ;
#8780 = AXIS2_PLACEMENT_3D('',#16398,#10460,#10461) ;
#8781 = AXIS2_PLACEMENT_3D('',#16400,#10463,#10464) ;
#8782 = AXIS2_PLACEMENT_3D('',#16404,#10465,#10466) ;
#8783 = AXIS2_PLACEMENT_3D('',#16412,#10469,#10470) ;
#8784 = AXIS2_PLACEMENT_3D('',#16414,#10472,#10473) ;
#8785 = AXIS2_PLACEMENT_3D('',#16418,#10474,#10475) ;
#8786 = AXIS2_PLACEMENT_3D('',#16426,#10478,#10479) ;
#8787 = AXIS2_PLACEMENT_3D('',#16428,#10481,#10482) ;
#8788 = AXIS2_PLACEMENT_3D('',#16432,#10483,#10484) ;
#8789 = AXIS2_PLACEMENT_3D('',#16440,#10487,#10488) ;
#8790 = AXIS2_PLACEMENT_3D('',#16442,#10490,#10491) ;
#8791 = AXIS2_PLACEMENT_3D('',#16446,#10492,#10493) ;
#8792 = AXIS2_PLACEMENT_3D('',#16454,#10496,#10497) ;
#8793 = AXIS2_PLACEMENT_3D('',#16456,#10499,#10500) ;
#8794 = AXIS2_PLACEMENT_3D('',#16460,#10501,#10502) ;
#8795 = AXIS2_PLACEMENT_3D('',#16468,#10505,#10506) ;
#8796 = AXIS2_PLACEMENT_3D('',#16470,#10508,#10509) ;
#8797 = AXIS2_PLACEMENT_3D('',#16474,#10510,#10511) ;
#8798 = AXIS2_PLACEMENT_3D('',#16482,#10514,#10515) ;
#8799 = AXIS2_PLACEMENT_3D('',#16484,#10517,#10518) ;
#8800 = AXIS2_PLACEMENT_3D('',#16488,#10519,#10520) ;
#8801 = AXIS2_PLACEMENT_3D('',#16496,#10523,#10524) ;
#8802 = AXIS2_PLACEMENT_3D('',#16498,#10526,#10527) ;
#8803 = AXIS2_PLACEMENT_3D('',#16502,#10528,#10529) ;
#8804 = AXIS2_PLACEMENT_3D('',#16510,#10532,#10533) ;
#8805 = AXIS2_PLACEMENT_3D('',#16512,#10535,#10536) ;
#8806 = AXIS2_PLACEMENT_3D('',#16516,#10537,#10538) ;
#8807 = AXIS2_PLACEMENT_3D('',#16524,#10541,#10542) ;
#8808 = AXIS2_PLACEMENT_3D('',#16526,#10544,#10545) ;
#8809 = AXIS2_PLACEMENT_3D('',#16530,#10546,#10547) ;
#8810 = AXIS2_PLACEMENT_3D('',#16538,#10550,#10551) ;
#8811 = AXIS2_PLACEMENT_3D('',#16540,#10553,#10554) ;
#8812 = AXIS2_PLACEMENT_3D('',#16544,#10555,#10556) ;
#8813 = AXIS2_PLACEMENT_3D('',#16552,#10559,#10560) ;
#8814 = AXIS2_PLACEMENT_3D('',#16554,#10562,#10563) ;
#8815 = AXIS2_PLACEMENT_3D('',#16558,#10564,#10565) ;
#8816 = AXIS2_PLACEMENT_3D('',#16566,#10568,#10569) ;
#8817 = AXIS2_PLACEMENT_3D('',#16568,#10571,#10572) ;
#8818 = AXIS2_PLACEMENT_3D('',#16572,#10573,#10574) ;
#8819 = AXIS2_PLACEMENT_3D('',#16580,#10577,#10578) ;
#8820 = AXIS2_PLACEMENT_3D('',#16582,#10580,#10581) ;
#8821 = AXIS2_PLACEMENT_3D('',#16586,#10582,#10583) ;
#8822 = AXIS2_PLACEMENT_3D('',#16594,#10586,#10587) ;
#8823 = AXIS2_PLACEMENT_3D('',#16596,#10589,#10590) ;
#8824 = AXIS2_PLACEMENT_3D('',#16600,#10591,#10592) ;
#8825 = AXIS2_PLACEMENT_3D('',#16608,#10595,#10596) ;
#8826 = AXIS2_PLACEMENT_3D('',#16610,#10598,#10599) ;
#8827 = AXIS2_PLACEMENT_3D('',#16614,#10600,#10601) ;
#8828 = AXIS2_PLACEMENT_3D('',#16615,#10602,#10603) ;
#8829 = AXIS2_PLACEMENT_3D('',#16616,#10604,#10605) ;
#8830 = AXIS2_PLACEMENT_3D('',#16618,#10606,#10607) ;
#8831 = AXIS2_PLACEMENT_3D('',#16620,#10609,#10610) ;
#8832 = AXIS2_PLACEMENT_3D('',#16622,#10611,#10612) ;
#8833 = AXIS2_PLACEMENT_3D('',#16623,#10613,#10614) ;
#8834 = AXIS2_PLACEMENT_3D('',#16630,#10615,#10616) ;
#8835 = AXIS2_PLACEMENT_3D('',#16640,#10617,#10618) ;
#8836 = AXIS2_PLACEMENT_3D('',#16650,#10619,#10620) ;
#8837 = AXIS2_PLACEMENT_3D('',#16660,#10621,#10622) ;
#8838 = AXIS2_PLACEMENT_3D('',#16670,#10623,#10624) ;
#8839 = AXIS2_PLACEMENT_3D('',#16681,#10626,#10627) ;
#8840 = AXIS2_PLACEMENT_3D('',#16685,#10628,#10629) ;
#8841 = AXIS2_PLACEMENT_3D('',#16690,#10632,#10633) ;
#8842 = AXIS2_PLACEMENT_3D('',#16691,#10634,#10635) ;
#8843 = AXIS2_PLACEMENT_3D('',#16695,#10637,#10638) ;
#8844 = AXIS2_PLACEMENT_3D('',#16697,#10640,#10641) ;
#8845 = AXIS2_PLACEMENT_3D('',#16702,#10644,#10645) ;
#8846 = AXIS2_PLACEMENT_3D('',#16703,#10646,#10647) ;
#8847 = AXIS2_PLACEMENT_3D('',#16707,#10649,#10650) ;
#8848 = AXIS2_PLACEMENT_3D('',#16709,#10652,#10653) ;
#8849 = AXIS2_PLACEMENT_3D('',#16714,#10656,#10657) ;
#8850 = AXIS2_PLACEMENT_3D('',#16715,#10658,#10659) ;
#8851 = AXIS2_PLACEMENT_3D('',#16719,#10661,#10662) ;
#8852 = AXIS2_PLACEMENT_3D('',#16721,#10664,#10665) ;
#8853 = AXIS2_PLACEMENT_3D('',#16728,#10670,#10671) ;
#8854 = AXIS2_PLACEMENT_3D('',#16733,#10675,#10676) ;
#8855 = AXIS2_PLACEMENT_3D('',#16738,#10680,#10681) ;
#8856 = AXIS2_PLACEMENT_3D('',#16739,#10682,#10683) ;
#8857 = AXIS2_PLACEMENT_3D('',#16740,#10684,#10685) ;
#8858 = AXIS2_PLACEMENT_3D('',#16742,#10687,#10688) ;
#8859 = AXIS2_PLACEMENT_3D('',#16743,#10689,#10690) ;
#8860 = AXIS2_PLACEMENT_3D('',#16745,#10692,#10693) ;
#8861 = AXIS2_PLACEMENT_3D('',#16747,#10695,#10696) ;
#8862 = AXIS2_PLACEMENT_3D('',#16751,#10698,#10699) ;
#8863 = AXIS2_PLACEMENT_3D('',#16752,#10700,#10701) ;
#8864 = AXIS2_PLACEMENT_3D('',#16754,#10703,#10704) ;
#8865 = AXIS2_PLACEMENT_3D('',#16755,#10705,#10706) ;
#8866 = AXIS2_PLACEMENT_3D('',#16756,#10707,#10708) ;
#8867 = AXIS2_PLACEMENT_3D('',#16757,#10709,#10710) ;
#8868 = AXIS2_PLACEMENT_3D('',#16758,#10711,#10712) ;
#8869 = AXIS2_PLACEMENT_3D('',#16759,#10713,#10714) ;
#8870 = AXIS2_PLACEMENT_3D('',#16760,#10715,#10716) ;
#8871 = AXIS2_PLACEMENT_3D('',#16761,#10717,#10718) ;
#8872 = AXIS2_PLACEMENT_3D('',#16763,#10720,#10721) ;
#8873 = AXIS2_PLACEMENT_3D('',#16764,#10722,#10723) ;
#8874 = AXIS2_PLACEMENT_3D('',#16767,#10725,#10726) ;
#8875 = AXIS2_PLACEMENT_3D('',#16770,#10729,#10730) ;
#8876 = AXIS2_PLACEMENT_3D('',#16771,#10731,#10732) ;
#8877 = AXIS2_PLACEMENT_3D('',#16772,#10733,#10734) ;
#8878 = AXIS2_PLACEMENT_3D('',#16773,#10735,#10736) ;
#8879 = AXIS2_PLACEMENT_3D('',#16775,#10737,#10738) ;
#8880 = AXIS2_PLACEMENT_3D('',#16777,#10739,#10740) ;
#8881 = AXIS2_PLACEMENT_3D('',#16778,#10741,#10742) ;
#8882 = AXIS2_PLACEMENT_3D('',#16780,#10743,#10744) ;
#8883 = AXIS2_PLACEMENT_3D('',#16782,#10746,#10747) ;
#8884 = AXIS2_PLACEMENT_3D('',#16784,#10748,#10749) ;
#8885 = AXIS2_PLACEMENT_3D('',#16785,#10750,#10751) ;
#8886 = AXIS2_PLACEMENT_3D('',#16788,#10753,#10754) ;
#8887 = AXIS2_PLACEMENT_3D('',#16789,#10755,#10756) ;
#8888 = AXIS2_PLACEMENT_3D('',#16792,#10758,#10759) ;
#8889 = AXIS2_PLACEMENT_3D('',#16793,#10760,#10761) ;
#8890 = AXIS2_PLACEMENT_3D('',#16796,#10763,#10764) ;
#8891 = AXIS2_PLACEMENT_3D('',#16797,#10765,#10766) ;
#8892 = AXIS2_PLACEMENT_3D('',#16800,#10768,#10769) ;
#8893 = AXIS2_PLACEMENT_3D('',#16801,#10770,#10771) ;
#8894 = AXIS2_PLACEMENT_3D('',#16804,#10773,#10774) ;
#8895 = AXIS2_PLACEMENT_3D('',#16805,#10775,#10776) ;
#8896 = AXIS2_PLACEMENT_3D('',#16807,#10778,#10779) ;
#8897 = AXIS2_PLACEMENT_3D('',#16808,#10780,#10781) ;
#8898 = AXIS2_PLACEMENT_3D('',#16810,#10782,#10783) ;
#8899 = AXIS2_PLACEMENT_3D('',#16813,#10785,#10786) ;
#8900 = AXIS2_PLACEMENT_3D('',#16814,#10787,#10788) ;
#8901 = AXIS2_PLACEMENT_3D('',#16823,#10793,#10794) ;
#8902 = AXIS2_PLACEMENT_3D('',#16829,#10798,#10799) ;
#8903 = AXIS2_PLACEMENT_3D('',#16835,#10803,#10804) ;
#8904 = AXIS2_PLACEMENT_3D('',#16837,#10805,#10806) ;
#8905 = AXIS2_PLACEMENT_3D('',#16844,#10810,#10811) ;
#8906 = AXIS2_PLACEMENT_3D('',#16846,#10812,#10813) ;
#8907 = AXIS2_PLACEMENT_3D('',#16847,#10814,#10815) ;
#8908 = AXIS2_PLACEMENT_3D('',#16849,#10816,#10817) ;
#8909 = AXIS2_PLACEMENT_3D('',#16851,#10819,#10820) ;
#8910 = AXIS2_PLACEMENT_3D('',#16857,#10824,#10825) ;
#8911 = AXIS2_PLACEMENT_3D('',#16861,#10828,#10829) ;
#8912 = AXIS2_PLACEMENT_3D('',#16862,#10830,#10831) ;
#8913 = AXIS2_PLACEMENT_3D('',#16863,#10832,#10833) ;
#8914 = AXIS2_PLACEMENT_3D('',#16867,#10836,#10837) ;
#8915 = AXIS2_PLACEMENT_3D('',#16868,#10838,#10839) ;
#8916 = AXIS2_PLACEMENT_3D('',#16869,#10840,#10841) ;
#8917 = AXIS2_PLACEMENT_3D('',#16870,#10842,#10843) ;
#8918 = AXIS2_PLACEMENT_3D('',#16871,#10844,#10845) ;
#8919 = AXIS2_PLACEMENT_3D('',#16872,#10846,#10847) ;
#8920 = AXIS2_PLACEMENT_3D('',#16873,#10848,#10849) ;
#8921 = AXIS2_PLACEMENT_3D('',#16874,#10850,#10851) ;
#8922 = AXIS2_PLACEMENT_3D('',#16875,#10852,#10853) ;
#8923 = AXIS2_PLACEMENT_3D('',#16876,#10854,#10855) ;
#8924 = AXIS2_PLACEMENT_3D('',#16877,#10856,#10857) ;
#8925 = AXIS2_PLACEMENT_3D('',#16878,#10858,#10859) ;
#8926 = AXIS2_PLACEMENT_3D('',#16879,#10860,#10861) ;
#8927 = AXIS2_PLACEMENT_3D('',#16880,#10862,#10863) ;
#8928 = AXIS2_PLACEMENT_3D('',#16881,#10864,#10865) ;
#8929 = AXIS2_PLACEMENT_3D('',#16882,#10866,#10867) ;
#8930 = AXIS2_PLACEMENT_3D('',#16883,#10868,#10869) ;
#8931 = AXIS2_PLACEMENT_3D('',#16884,#10870,#10871) ;
#8932 = AXIS2_PLACEMENT_3D('',#16885,#10872,#10873) ;
#8933 = AXIS2_PLACEMENT_3D('',#16886,#10874,#10875) ;
#8934 = AXIS2_PLACEMENT_3D('',#16887,#10876,#10877) ;
#8935 = AXIS2_PLACEMENT_3D('',#16888,#10878,#10879) ;
#8936 = AXIS2_PLACEMENT_3D('',#16889,#10880,#10881) ;
#8937 = AXIS2_PLACEMENT_3D('',#16890,#10882,#10883) ;
#8938 = AXIS2_PLACEMENT_3D('',#16891,#10884,#10885) ;
#8939 = AXIS2_PLACEMENT_3D('',#16892,#10886,#10887) ;
#8940 = AXIS2_PLACEMENT_3D('',#16893,#10888,#10889) ;
#8941 = AXIS2_PLACEMENT_3D('',#16894,#10890,#10891) ;
#8942 = AXIS2_PLACEMENT_3D('',#16895,#10892,#10893) ;
#8943 = AXIS2_PLACEMENT_3D('',#16896,#10894,#10895) ;
#8944 = AXIS2_PLACEMENT_3D('',#16897,#10896,#10897) ;
#8945 = AXIS2_PLACEMENT_3D('',#16898,#10898,#10899) ;
#8946 = AXIS2_PLACEMENT_3D('',#16899,#10900,#10901) ;
#8947 = AXIS2_PLACEMENT_3D('',#16900,#10902,#10903) ;
#8948 = AXIS2_PLACEMENT_3D('',#16901,#10904,#10905) ;
#8949 = AXIS2_PLACEMENT_3D('',#16902,#10906,#10907) ;
#8950 = AXIS2_PLACEMENT_3D('',#16903,#10908,#10909) ;
#8951 = AXIS2_PLACEMENT_3D('',#16904,#10910,#10911) ;
#8952 = AXIS2_PLACEMENT_3D('',#16905,#10912,#10913) ;
#8953 = AXIS2_PLACEMENT_3D('',#16906,#10914,#10915) ;
#8954 = AXIS2_PLACEMENT_3D('',#16907,#10916,#10917) ;
#8955 = AXIS2_PLACEMENT_3D('',#16908,#10918,#10919) ;
#8956 = AXIS2_PLACEMENT_3D('',#16909,#10920,#10921) ;
#8957 = AXIS2_PLACEMENT_3D('',#16910,#10922,#10923) ;
#8958 = AXIS2_PLACEMENT_3D('',#16911,#10924,#10925) ;
#8959 = AXIS2_PLACEMENT_3D('',#16912,#10926,#10927) ;
#8960 = AXIS2_PLACEMENT_3D('',#16913,#10928,#10929) ;
#8961 = AXIS2_PLACEMENT_3D('',#16914,#10930,#10931) ;
#8962 = AXIS2_PLACEMENT_3D('',#16915,#10932,#10933) ;
#8963 = AXIS2_PLACEMENT_3D('',#16916,#10934,#10935) ;
#8964 = AXIS2_PLACEMENT_3D('',#16917,#10936,#10937) ;
#8965 = AXIS2_PLACEMENT_3D('',#16918,#10938,#10939) ;
#8966 = AXIS2_PLACEMENT_3D('',#16919,#10940,#10941) ;
#8967 = AXIS2_PLACEMENT_3D('',#16920,#10942,#10943) ;
#8968 = AXIS2_PLACEMENT_3D('',#16921,#10944,#10945) ;
#8969 = AXIS2_PLACEMENT_3D('',#16922,#10946,#10947) ;
#8970 = AXIS2_PLACEMENT_3D('',#16923,#10948,#10949) ;
#8971 = AXIS2_PLACEMENT_3D('',#16924,#10950,#10951) ;
#8972 = DIRECTION('axis',(0.,0.,1.)) ;
#8973 = DIRECTION('refdir',(1.,0.,0.)) ;
#8974 = DIRECTION('axis',(0.,0.,1.)) ;
#8975 = DIRECTION('refdir',(1.,0.,0.)) ;
#8976 = DIRECTION('center_axis',(1.,0.,0.)) ;
#8977 = DIRECTION('ref_axis',(0.,0.,-1.)) ;
#8978 = DIRECTION('center_axis',(1.,0.,0.)) ;
#8979 = DIRECTION('ref_axis',(0.,0.,-1.)) ;
#8980 = DIRECTION('',(-0.707106781186554,8.65956056235486E-17,-0.707106781186541)) ;
#8981 = DIRECTION('center_axis',(-1.,0.,0.)) ;
#8982 = DIRECTION('ref_axis',(0.,0.,-1.)) ;
#8983 = DIRECTION('center_axis',(-1.,0.,0.)) ;
#8984 = DIRECTION('ref_axis',(0.,0.,-1.)) ;
#8985 = DIRECTION('',(-1.,0.,0.)) ;
#8986 = DIRECTION('center_axis',(-1.,0.,0.)) ;
#8987 = DIRECTION('ref_axis',(0.,0.,-1.)) ;
#8988 = DIRECTION('center_axis',(-1.,0.,0.)) ;
#8989 = DIRECTION('ref_axis',(0.,0.,-1.)) ;
#8990 = DIRECTION('center_axis',(1.,0.,0.)) ;
#8991 = DIRECTION('ref_axis',(0.,0.,-1.)) ;
#8992 = DIRECTION('center_axis',(1.,0.,0.)) ;
#8993 = DIRECTION('ref_axis',(0.,0.,-1.)) ;
#8994 = DIRECTION('center_axis',(1.,0.,0.)) ;
#8995 = DIRECTION('ref_axis',(0.,1.,0.)) ;
#8996 = DIRECTION('',(0.515038074910055,-0.857167300702112,-1.04972719113862E-16)) ;
#8997 = DIRECTION('center_axis',(-1.,0.,0.)) ;
#8998 = DIRECTION('ref_axis',(0.,0.,-1.)) ;
#8999 = DIRECTION('center_axis',(-1.,0.,0.)) ;
#9000 = DIRECTION('ref_axis',(0.,0.,-1.)) ;
#9001 = DIRECTION('',(0.707106781186549,-8.65956056235492E-17,-0.707106781186546)) ;
#9002 = DIRECTION('center_axis',(1.,0.,0.)) ;
#9003 = DIRECTION('ref_axis',(0.,0.,-1.)) ;
#9004 = DIRECTION('center_axis',(1.,0.,0.)) ;
#9005 = DIRECTION('ref_axis',(0.,0.,-1.)) ;
#9006 = DIRECTION('',(1.,0.,0.)) ;
#9007 = DIRECTION('center_axis',(1.,0.,0.)) ;
#9008 = DIRECTION('ref_axis',(0.,0.,-1.)) ;
#9009 = DIRECTION('center_axis',(1.,0.,0.)) ;
#9010 = DIRECTION('ref_axis',(0.,0.,-1.)) ;
#9011 = DIRECTION('center_axis',(-1.,0.,0.)) ;
#9012 = DIRECTION('ref_axis',(0.,0.,1.)) ;
#9013 = DIRECTION('center_axis',(1.,0.,0.)) ;
#9014 = DIRECTION('ref_axis',(0.,0.,-1.)) ;
#9015 = DIRECTION('center_axis',(-1.,0.,0.)) ;
#9016 = DIRECTION('ref_axis',(0.,1.,0.)) ;
#9017 = DIRECTION('',(0.515038074910053,0.857167300702113,1.04972719113862E-16)) ;
#9018 = DIRECTION('center_axis',(1.,0.,0.)) ;
#9019 = DIRECTION('ref_axis',(0.,0.,-1.)) ;
#9020 = DIRECTION('center_axis',(1.,0.,0.)) ;
#9021 = DIRECTION('ref_axis',(0.,1.,0.)) ;
#9022 = DIRECTION('',(0.,0.,1.)) ;
#9023 = DIRECTION('center_axis',(1.,0.,0.)) ;
#9024 = DIRECTION('ref_axis',(0.,1.,0.)) ;
#9025 = DIRECTION('center_axis',(0.,1.,0.)) ;
#9026 = DIRECTION('ref_axis',(0.,0.,1.)) ;
#9027 = DIRECTION('',(1.,0.,0.)) ;
#9028 = DIRECTION('',(0.,0.,-1.)) ;
#9029 = DIRECTION('',(-1.,0.,0.)) ;
#9030 = DIRECTION('center_axis',(1.,0.,0.)) ;
#9031 = DIRECTION('ref_axis',(0.,0.,-1.)) ;
#9032 = DIRECTION('center_axis',(-1.,0.,0.)) ;
#9033 = DIRECTION('ref_axis',(0.,1.,0.)) ;
#9034 = DIRECTION('center_axis',(-1.,0.,0.)) ;
#9035 = DIRECTION('ref_axis',(0.,1.,0.)) ;
#9036 = DIRECTION('center_axis',(1.,0.,0.)) ;
#9037 = DIRECTION('ref_axis',(0.,0.,-1.)) ;
#9038 = DIRECTION('center_axis',(-1.,0.,0.)) ;
#9039 = DIRECTION('ref_axis',(0.,1.,0.)) ;
#9040 = DIRECTION('',(0.,0.,-1.)) ;
#9041 = DIRECTION('center_axis',(0.,-1.,0.)) ;
#9042 = DIRECTION('ref_axis',(0.,0.,-1.)) ;
#9043 = DIRECTION('',(-1.,0.,0.)) ;
#9044 = DIRECTION('',(0.,0.,-1.)) ;
#9045 = DIRECTION('',(1.,0.,0.)) ;
#9046 = DIRECTION('center_axis',(1.,0.,0.)) ;
#9047 = DIRECTION('ref_axis',(0.,0.,-1.)) ;
#9048 = DIRECTION('center_axis',(1.,0.,0.)) ;
#9049 = DIRECTION('ref_axis',(0.,1.,0.)) ;
#9050 = DIRECTION('center_axis',(1.,0.,0.)) ;
#9051 = DIRECTION('ref_axis',(0.,0.707106781186547,0.707106781186548)) ;
#9052 = DIRECTION('center_axis',(-1.,0.,0.)) ;
#9053 = DIRECTION('ref_axis',(0.,0.,-1.)) ;
#9054 = DIRECTION('',(1.,0.,0.)) ;
#9055 = DIRECTION('center_axis',(1.,0.,0.)) ;
#9056 = DIRECTION('ref_axis',(0.,0.,-1.)) ;
#9057 = DIRECTION('',(-1.,0.,0.)) ;
#9058 = DIRECTION('center_axis',(1.,0.,0.)) ;
#9059 = DIRECTION('ref_axis',(0.,-0.707106781186547,0.707106781186548)) ;
#9060 = DIRECTION('center_axis',(-1.,0.,0.)) ;
#9061 = DIRECTION('ref_axis',(0.,0.,-1.)) ;
#9062 = DIRECTION('',(1.,0.,0.)) ;
#9063 = DIRECTION('center_axis',(1.,0.,0.)) ;
#9064 = DIRECTION('ref_axis',(0.,0.,-1.)) ;
#9065 = DIRECTION('',(-1.,0.,0.)) ;
#9066 = DIRECTION('center_axis',(1.,0.,0.)) ;
#9067 = DIRECTION('ref_axis',(0.,0.,-1.)) ;
#9068 = DIRECTION('',(1.,0.,0.)) ;
#9069 = DIRECTION('center_axis',(1.,0.,0.)) ;
#9070 = DIRECTION('ref_axis',(0.,0.,-1.)) ;
#9071 = DIRECTION('',(-1.,0.,0.)) ;
#9072 = DIRECTION('center_axis',(-1.,0.,0.)) ;
#9073 = DIRECTION('ref_axis',(0.,0.,-1.)) ;
#9074 = DIRECTION('center_axis',(1.,0.,0.)) ;
#9075 = DIRECTION('ref_axis',(0.,0.,-1.)) ;
#9076 = DIRECTION('',(1.,0.,0.)) ;
#9077 = DIRECTION('center_axis',(1.,0.,0.)) ;
#9078 = DIRECTION('ref_axis',(0.,0.,-1.)) ;
#9079 = DIRECTION('',(-1.,0.,0.)) ;
#9080 = DIRECTION('center_axis',(-1.,0.,0.)) ;
#9081 = DIRECTION('ref_axis',(0.,0.,-1.)) ;
#9082 = DIRECTION('center_axis',(-1.,0.,0.)) ;
#9083 = DIRECTION('ref_axis',(0.,1.,0.)) ;
#9084 = DIRECTION('center_axis',(1.,0.,0.)) ;
#9085 = DIRECTION('ref_axis',(0.,0.,-1.)) ;
#9086 = DIRECTION('center_axis',(1.,0.,0.)) ;
#9087 = DIRECTION('ref_axis',(0.,0.,-1.)) ;
#9088 = DIRECTION('center_axis',(-1.,0.,0.)) ;
#9089 = DIRECTION('ref_axis',(0.,1.,0.)) ;
#9090 = DIRECTION('center_axis',(1.,0.,0.)) ;
#9091 = DIRECTION('ref_axis',(0.,0.,-1.)) ;
#9092 = DIRECTION('center_axis',(1.,0.,0.)) ;
#9093 = DIRECTION('ref_axis',(0.,0.,-1.)) ;
#9094 = DIRECTION('center_axis',(-1.,0.,0.)) ;
#9095 = DIRECTION('ref_axis',(0.,-1.,-1.01064309961486E-15)) ;
#9096 = DIRECTION('center_axis',(1.,0.,0.)) ;
#9097 = DIRECTION('ref_axis',(0.,0.,-1.)) ;
#9098 = DIRECTION('center_axis',(1.,0.,0.)) ;
#9099 = DIRECTION('ref_axis',(0.,0.,-1.)) ;
#9100 = DIRECTION('center_axis',(-1.,0.,0.)) ;
#9101 = DIRECTION('ref_axis',(0.,1.,0.)) ;
#9102 = DIRECTION('center_axis',(1.,0.,0.)) ;
#9103 = DIRECTION('ref_axis',(0.,0.,-1.)) ;
#9104 = DIRECTION('center_axis',(1.,0.,0.)) ;
#9105 = DIRECTION('ref_axis',(0.,0.,-1.)) ;
#9106 = DIRECTION('center_axis',(1.,0.,0.)) ;
#9107 = DIRECTION('ref_axis',(0.,1.,0.)) ;
#9108 = DIRECTION('center_axis',(1.,0.,0.)) ;
#9109 = DIRECTION('ref_axis',(0.,0.,-1.)) ;
#9110 = DIRECTION('center_axis',(1.,0.,0.)) ;
#9111 = DIRECTION('ref_axis',(0.,1.,0.)) ;
#9112 = DIRECTION('center_axis',(1.,0.,0.)) ;
#9113 = DIRECTION('ref_axis',(0.,0.,-1.)) ;
#9114 = DIRECTION('center_axis',(1.,0.,0.)) ;
#9115 = DIRECTION('ref_axis',(0.,-1.,-1.01064309961486E-15)) ;
#9116 = DIRECTION('center_axis',(1.,0.,0.)) ;
#9117 = DIRECTION('ref_axis',(0.,0.,-1.)) ;
#9118 = DIRECTION('center_axis',(1.,0.,0.)) ;
#9119 = DIRECTION('ref_axis',(0.,1.,0.)) ;
#9120 = DIRECTION('center_axis',(1.,0.,0.)) ;
#9121 = DIRECTION('ref_axis',(0.,0.,-1.)) ;
#9122 = DIRECTION('center_axis',(1.,0.,0.)) ;
#9123 = DIRECTION('ref_axis',(0.,1.,0.)) ;
#9124 = DIRECTION('center_axis',(1.,0.,0.)) ;
#9125 = DIRECTION('ref_axis',(0.,0.,-1.)) ;
#9126 = DIRECTION('center_axis',(1.,0.,0.)) ;
#9127 = DIRECTION('ref_axis',(0.,1.,0.)) ;
#9128 = DIRECTION('center_axis',(1.,0.,0.)) ;
#9129 = DIRECTION('ref_axis',(0.,0.,-1.)) ;
#9130 = DIRECTION('center_axis',(1.,0.,0.)) ;
#9131 = DIRECTION('ref_axis',(0.,-1.,-1.01064309961486E-15)) ;
#9132 = DIRECTION('center_axis',(1.,0.,0.)) ;
#9133 = DIRECTION('ref_axis',(0.,0.,-1.)) ;
#9134 = DIRECTION('center_axis',(1.,0.,0.)) ;
#9135 = DIRECTION('ref_axis',(0.,1.,0.)) ;
#9136 = DIRECTION('center_axis',(1.,0.,0.)) ;
#9137 = DIRECTION('ref_axis',(0.,0.,-1.)) ;
#9138 = DIRECTION('center_axis',(-1.,0.,0.)) ;
#9139 = DIRECTION('ref_axis',(0.,0.,1.)) ;
#9140 = DIRECTION('center_axis',(1.,0.,0.)) ;
#9141 = DIRECTION('ref_axis',(0.,0.,-1.)) ;
#9142 = DIRECTION('center_axis',(1.,0.,0.)) ;
#9143 = DIRECTION('ref_axis',(0.,1.,0.)) ;
#9144 = DIRECTION('center_axis',(1.,0.,0.)) ;
#9145 = DIRECTION('ref_axis',(0.,0.,-1.)) ;
#9146 = DIRECTION('',(-0.707106781186549,0.707106781186546,8.65956056235492E-17)) ;
#9147 = DIRECTION('center_axis',(1.,0.,0.)) ;
#9148 = DIRECTION('ref_axis',(0.,1.,0.)) ;
#9149 = DIRECTION('',(-1.,0.,0.)) ;
#9150 = DIRECTION('center_axis',(1.,0.,0.)) ;
#9151 = DIRECTION('ref_axis',(0.,0.,-1.)) ;
#9152 = DIRECTION('center_axis',(1.,0.,0.)) ;
#9153 = DIRECTION('ref_axis',(0.,0.,-1.)) ;
#9154 = DIRECTION('center_axis',(1.,0.,0.)) ;
#9155 = DIRECTION('ref_axis',(0.,1.,0.)) ;
#9156 = DIRECTION('center_axis',(1.,0.,0.)) ;
#9157 = DIRECTION('ref_axis',(0.,0.,-1.)) ;
#9158 = DIRECTION('',(-1.,0.,0.)) ;
#9159 = DIRECTION('',(-1.,0.,0.)) ;
#9160 = DIRECTION('center_axis',(-1.,0.,0.)) ;
#9161 = DIRECTION('ref_axis',(0.,1.,0.)) ;
#9162 = DIRECTION('',(-0.707106781186554,-0.707106781186541,-8.65956056235486E-17)) ;
#9163 = DIRECTION('axis',(0.,0.,1.)) ;
#9164 = DIRECTION('refdir',(1.,0.,0.)) ;
#9165 = DIRECTION('',(0.,-1.,0.)) ;
#9166 = DIRECTION('',(0.,-1.,0.)) ;
#9167 = DIRECTION('',(0.,-1.,0.)) ;
#9168 = DIRECTION('',(0.,-1.,0.)) ;
#9169 = DIRECTION('',(0.,-1.,0.)) ;
#9170 = DIRECTION('',(0.,-1.,0.)) ;
#9171 = DIRECTION('',(0.,-1.,0.)) ;
#9172 = DIRECTION('',(0.,-1.,0.)) ;
#9173 = DIRECTION('',(0.,-1.,0.)) ;
#9174 = DIRECTION('',(0.,-1.,0.)) ;
#9175 = DIRECTION('',(0.,-1.,0.)) ;
#9176 = DIRECTION('',(0.,-1.,0.)) ;
#9177 = DIRECTION('',(0.,-1.,0.)) ;
#9178 = DIRECTION('',(0.,-1.,0.)) ;
#9179 = DIRECTION('',(0.,-1.,0.)) ;
#9180 = DIRECTION('',(0.,-1.,0.)) ;
#9181 = DIRECTION('',(0.,-1.,0.)) ;
#9182 = DIRECTION('',(0.,-1.,0.)) ;
#9183 = DIRECTION('',(0.,-1.,0.)) ;
#9184 = DIRECTION('',(0.,-1.,0.)) ;
#9185 = DIRECTION('',(0.,-1.,0.)) ;
#9186 = DIRECTION('',(0.,-1.,0.)) ;
#9187 = DIRECTION('',(0.,-1.,0.)) ;
#9188 = DIRECTION('',(0.,-1.,0.)) ;
#9189 = DIRECTION('',(0.,-1.,0.)) ;
#9190 = DIRECTION('',(0.,-1.,0.)) ;
#9191 = DIRECTION('',(0.,-1.,0.)) ;
#9192 = DIRECTION('center_axis',(0.0779742589964975,0.,0.996955372588938)) ;
#9193 = DIRECTION('ref_axis',(-0.996955372588938,0.,0.0779742589964975)) ;
#9194 = DIRECTION('center_axis',(0.0779742589964975,0.,0.996955372588938)) ;
#9195 = DIRECTION('ref_axis',(-0.996955372588938,0.,0.0779742589964975)) ;
#9196 = DIRECTION('',(0.,-1.,0.)) ;
#9197 = DIRECTION('',(-0.996955372588938,0.,0.0779742589964975)) ;
#9198 = DIRECTION('center_axis',(0.,1.,0.)) ;
#9199 = DIRECTION('ref_axis',(1.,0.,0.)) ;
#9200 = DIRECTION('',(0.,-1.,0.)) ;
#9201 = DIRECTION('',(0.,-1.,0.)) ;
#9202 = DIRECTION('center_axis',(-1.,0.,0.)) ;
#9203 = DIRECTION('ref_axis',(0.,0.,-1.)) ;
#9204 = DIRECTION('center_axis',(-1.,0.,0.)) ;
#9205 = DIRECTION('ref_axis',(0.,1.,0.)) ;
#9206 = DIRECTION('',(0.,0.,-1.)) ;
#9207 = DIRECTION('',(0.,-1.,0.)) ;
#9208 = DIRECTION('',(0.,-1.,0.)) ;
#9209 = DIRECTION('',(0.,-1.,0.)) ;
#9210 = DIRECTION('center_axis',(0.,0.,-1.)) ;
#9211 = DIRECTION('ref_axis',(1.,0.,0.)) ;
#9212 = DIRECTION('',(1.,0.,0.)) ;
#9213 = DIRECTION('',(1.,0.,0.)) ;
#9214 = DIRECTION('',(0.,-1.,0.)) ;
#9215 = DIRECTION('',(0.,-1.,0.)) ;
#9216 = DIRECTION('center_axis',(-1.,0.,0.)) ;
#9217 = DIRECTION('ref_axis',(0.,0.,-1.)) ;
#9218 = DIRECTION('center_axis',(-1.,0.,0.)) ;
#9219 = DIRECTION('ref_axis',(0.,1.,0.)) ;
#9220 = DIRECTION('',(0.,-1.,0.)) ;
#9221 = DIRECTION('',(0.,0.,-1.)) ;
#9222 = DIRECTION('center_axis',(0.,0.,1.)) ;
#9223 = DIRECTION('ref_axis',(-1.,0.,0.)) ;
#9224 = DIRECTION('',(-1.,0.,0.)) ;
#9225 = DIRECTION('',(0.,-1.,0.)) ;
#9226 = DIRECTION('',(-1.,0.,0.)) ;
#9227 = DIRECTION('center_axis',(1.,0.,0.)) ;
#9228 = DIRECTION('ref_axis',(0.,0.,1.)) ;
#9229 = DIRECTION('center_axis',(1.,0.,0.)) ;
#9230 = DIRECTION('ref_axis',(0.,1.,0.)) ;
#9231 = DIRECTION('',(0.,0.,1.)) ;
#9232 = DIRECTION('center_axis',(0.,1.,0.)) ;
#9233 = DIRECTION('ref_axis',(1.,0.,0.)) ;
#9234 = DIRECTION('center_axis',(1.,0.,0.)) ;
#9235 = DIRECTION('ref_axis',(0.,1.,0.)) ;
#9236 = DIRECTION('center_axis',(1.,0.,0.)) ;
#9237 = DIRECTION('ref_axis',(0.,0.,-1.)) ;
#9238 = DIRECTION('',(-1.,0.,0.)) ;
#9239 = DIRECTION('center_axis',(1.,0.,0.)) ;
#9240 = DIRECTION('ref_axis',(0.,1.,0.)) ;
#9241 = DIRECTION('center_axis',(1.,0.,0.)) ;
#9242 = DIRECTION('ref_axis',(0.,1.,0.)) ;
#9243 = DIRECTION('',(-1.,0.,0.)) ;
#9244 = DIRECTION('center_axis',(-1.,0.,0.)) ;
#9245 = DIRECTION('ref_axis',(0.,1.,0.)) ;
#9246 = DIRECTION('',(1.,0.,0.)) ;
#9247 = DIRECTION('center_axis',(0.948408846174048,0.,-0.317049933762509)) ;
#9248 = DIRECTION('ref_axis',(0.317049933762509,0.,0.948408846174048)) ;
#9249 = DIRECTION('center_axis',(-0.945579694085495,0.,-0.325390599331299)) ;
#9250 = DIRECTION('ref_axis',(-0.325390599331299,0.,0.945579694085495)) ;
#9251 = DIRECTION('',(1.,0.,0.)) ;
#9252 = DIRECTION('center_axis',(1.,0.,0.)) ;
#9253 = DIRECTION('ref_axis',(0.,1.,0.)) ;
#9254 = DIRECTION('',(-1.,0.,0.)) ;
#9255 = DIRECTION('center_axis',(-1.,0.,0.)) ;
#9256 = DIRECTION('ref_axis',(0.,1.,0.)) ;
#9257 = DIRECTION('center_axis',(0.944683590425841,0.,0.327983100144111)) ;
#9258 = DIRECTION('ref_axis',(-0.327983100144111,0.,0.944683590425841)) ;
#9259 = DIRECTION('',(-1.,0.,0.)) ;
#9260 = DIRECTION('center_axis',(-0.946846702516136,0.,0.321685128556358)) ;
#9261 = DIRECTION('ref_axis',(0.321685128556358,0.,0.946846702516135)) ;
#9262 = DIRECTION('center_axis',(-0.0870991451328652,0.,-0.996199648121361)) ;
#9263 = DIRECTION('ref_axis',(-0.996199648121361,0.,0.0870991451328652)) ;
#9264 = DIRECTION('center_axis',(0.0750566132645402,0.,0.997179274155484)) ;
#9265 = DIRECTION('ref_axis',(-0.997179274155484,0.,0.0750566132645402)) ;
#9266 = DIRECTION('center_axis',(-1.,0.,0.)) ;
#9267 = DIRECTION('ref_axis',(0.,1.,0.)) ;
#9268 = DIRECTION('',(1.,0.,0.)) ;
#9269 = DIRECTION('center_axis',(1.,0.,0.)) ;
#9270 = DIRECTION('ref_axis',(0.,1.,0.)) ;
#9271 = DIRECTION('center_axis',(-1.,0.,0.)) ;
#9272 = DIRECTION('ref_axis',(0.,1.,0.)) ;
#9273 = DIRECTION('',(1.,0.,0.)) ;
#9274 = DIRECTION('center_axis',(1.,0.,0.)) ;
#9275 = DIRECTION('ref_axis',(0.,1.,0.)) ;
#9276 = DIRECTION('center_axis',(1.,0.,0.)) ;
#9277 = DIRECTION('ref_axis',(0.,1.,0.)) ;
#9278 = DIRECTION('',(-1.,0.,0.)) ;
#9279 = DIRECTION('center_axis',(-1.,0.,0.)) ;
#9280 = DIRECTION('ref_axis',(0.,1.,0.)) ;
#9281 = DIRECTION('',(1.,0.,0.)) ;
#9282 = DIRECTION('center_axis',(0.948408859814315,0.,-0.317049892959627)) ;
#9283 = DIRECTION('ref_axis',(0.317049892959627,0.,0.948408859814315)) ;
#9284 = DIRECTION('center_axis',(-0.945579694085495,0.,-0.325390599331299)) ;
#9285 = DIRECTION('ref_axis',(-0.325390599331299,0.,0.945579694085495)) ;
#9286 = DIRECTION('',(1.,0.,0.)) ;
#9287 = DIRECTION('center_axis',(1.,0.,0.)) ;
#9288 = DIRECTION('ref_axis',(0.,1.,0.)) ;
#9289 = DIRECTION('',(-1.,0.,0.)) ;
#9290 = DIRECTION('center_axis',(-1.,0.,0.)) ;
#9291 = DIRECTION('ref_axis',(0.,1.,0.)) ;
#9292 = DIRECTION('center_axis',(0.944683566738785,0.,0.327983168369488)) ;
#9293 = DIRECTION('ref_axis',(-0.327983168369488,0.,0.944683566738785)) ;
#9294 = DIRECTION('',(-1.,0.,0.)) ;
#9295 = DIRECTION('center_axis',(-0.946846725462142,0.,0.321685061017167)) ;
#9296 = DIRECTION('ref_axis',(0.321685061017167,0.,0.946846725462142)) ;
#9297 = DIRECTION('center_axis',(1.,0.,0.)) ;
#9298 = DIRECTION('ref_axis',(0.,1.,0.)) ;
#9299 = DIRECTION('',(-1.,0.,0.)) ;
#9300 = DIRECTION('center_axis',(-1.,0.,0.)) ;
#9301 = DIRECTION('ref_axis',(0.,1.,0.)) ;
#9302 = DIRECTION('',(1.,0.,0.)) ;
#9303 = DIRECTION('center_axis',(1.,0.,0.)) ;
#9304 = DIRECTION('ref_axis',(0.,1.,0.)) ;
#9305 = DIRECTION('',(-1.,0.,0.)) ;
#9306 = DIRECTION('center_axis',(-1.,0.,0.)) ;
#9307 = DIRECTION('ref_axis',(0.,1.,0.)) ;
#9308 = DIRECTION('',(1.,0.,0.)) ;
#9309 = DIRECTION('center_axis',(-1.,0.,0.)) ;
#9310 = DIRECTION('ref_axis',(0.,0.,-1.)) ;
#9311 = DIRECTION('',(0.,-1.,0.)) ;
#9312 = DIRECTION('',(0.,0.,-1.)) ;
#9313 = DIRECTION('',(0.,-1.,0.)) ;
#9314 = DIRECTION('center_axis',(0.,0.,-1.)) ;
#9315 = DIRECTION('ref_axis',(1.,0.,0.)) ;
#9316 = DIRECTION('',(1.,0.,0.)) ;
#9317 = DIRECTION('',(0.,-1.,0.)) ;
#9318 = DIRECTION('center_axis',(1.,0.,0.)) ;
#9319 = DIRECTION('ref_axis',(0.,0.,1.)) ;
#9320 = DIRECTION('',(0.,0.,1.)) ;
#9321 = DIRECTION('',(0.,-1.,0.)) ;
#9322 = DIRECTION('center_axis',(0.,0.,1.)) ;
#9323 = DIRECTION('ref_axis',(-1.,0.,0.)) ;
#9324 = DIRECTION('',(-1.,0.,0.)) ;
#9325 = DIRECTION('center_axis',(0.,-1.,0.)) ;
#9326 = DIRECTION('ref_axis',(0.,0.,-1.)) ;
#9327 = DIRECTION('center_axis',(-1.,0.,0.)) ;
#9328 = DIRECTION('ref_axis',(0.,0.,-1.)) ;
#9329 = DIRECTION('',(0.,-1.,0.)) ;
#9330 = DIRECTION('',(0.,0.,-1.)) ;
#9331 = DIRECTION('',(0.,-1.,0.)) ;
#9332 = DIRECTION('center_axis',(0.,0.,-1.)) ;
#9333 = DIRECTION('ref_axis',(1.,0.,0.)) ;
#9334 = DIRECTION('',(1.,0.,0.)) ;
#9335 = DIRECTION('',(0.,-1.,0.)) ;
#9336 = DIRECTION('center_axis',(1.,0.,0.)) ;
#9337 = DIRECTION('ref_axis',(0.,0.,1.)) ;
#9338 = DIRECTION('',(0.,0.,1.)) ;
#9339 = DIRECTION('',(0.,-1.,0.)) ;
#9340 = DIRECTION('center_axis',(0.,0.,1.)) ;
#9341 = DIRECTION('ref_axis',(-1.,0.,0.)) ;
#9342 = DIRECTION('',(-1.,0.,0.)) ;
#9343 = DIRECTION('center_axis',(0.,-1.,0.)) ;
#9344 = DIRECTION('ref_axis',(0.,0.,-1.)) ;
#9345 = DIRECTION('center_axis',(0.,0.,-1.)) ;
#9346 = DIRECTION('ref_axis',(1.,0.,0.)) ;
#9347 = DIRECTION('',(0.,-1.,0.)) ;
#9348 = DIRECTION('',(1.,0.,0.)) ;
#9349 = DIRECTION('',(0.,-1.,0.)) ;
#9350 = DIRECTION('center_axis',(1.,0.,0.)) ;
#9351 = DIRECTION('ref_axis',(0.,0.,1.)) ;
#9352 = DIRECTION('',(0.,0.,1.)) ;
#9353 = DIRECTION('',(0.,-1.,0.)) ;
#9354 = DIRECTION('center_axis',(0.,0.,1.)) ;
#9355 = DIRECTION('ref_axis',(-1.,0.,0.)) ;
#9356 = DIRECTION('',(-1.,0.,0.)) ;
#9357 = DIRECTION('',(0.,-1.,0.)) ;
#9358 = DIRECTION('center_axis',(-1.,0.,0.)) ;
#9359 = DIRECTION('ref_axis',(0.,0.,-1.)) ;
#9360 = DIRECTION('',(0.,0.,-1.)) ;
#9361 = DIRECTION('',(0.,-1.,0.)) ;
#9362 = DIRECTION('center_axis',(0.944683566738785,0.,0.327983168369488)) ;
#9363 = DIRECTION('ref_axis',(-0.327983168369488,0.,0.944683566738785)) ;
#9364 = DIRECTION('',(-0.327983168369488,0.,0.944683566738785)) ;
#9365 = DIRECTION('',(0.,-1.,0.)) ;
#9366 = DIRECTION('center_axis',(0.,0.,1.)) ;
#9367 = DIRECTION('ref_axis',(-1.,0.,0.)) ;
#9368 = DIRECTION('',(-1.,0.,0.)) ;
#9369 = DIRECTION('',(0.,-1.,0.)) ;
#9370 = DIRECTION('center_axis',(-0.946846725462142,0.,0.321685061017167)) ;
#9371 = DIRECTION('ref_axis',(-0.321685061017167,0.,-0.946846725462142)) ;
#9372 = DIRECTION('',(-0.321685061017167,0.,-0.946846725462142)) ;
#9373 = DIRECTION('',(0.,-1.,0.)) ;
#9374 = DIRECTION('center_axis',(1.,0.,0.)) ;
#9375 = DIRECTION('ref_axis',(0.,0.,1.)) ;
#9376 = DIRECTION('',(0.,0.,1.)) ;
#9377 = DIRECTION('',(0.,-1.,0.)) ;
#9378 = DIRECTION('center_axis',(-0.945579694085495,0.,-0.325390599331299)) ;
#9379 = DIRECTION('ref_axis',(0.325390599331299,0.,-0.945579694085495)) ;
#9380 = DIRECTION('',(0.,-1.,0.)) ;
#9381 = DIRECTION('',(0.325390599331299,0.,-0.945579694085495)) ;
#9382 = DIRECTION('',(0.,-1.,0.)) ;
#9383 = DIRECTION('',(0.,-1.,0.)) ;
#9384 = DIRECTION('center_axis',(0.948408859814315,0.,-0.317049892959627)) ;
#9385 = DIRECTION('ref_axis',(0.317049892959627,0.,0.948408859814315)) ;
#9386 = DIRECTION('',(0.,-1.,0.)) ;
#9387 = DIRECTION('',(0.317049892959627,0.,0.948408859814315)) ;
#9388 = DIRECTION('center_axis',(0.,0.,-1.)) ;
#9389 = DIRECTION('ref_axis',(1.,0.,0.)) ;
#9390 = DIRECTION('',(0.,-1.,0.)) ;
#9391 = DIRECTION('',(1.,0.,0.)) ;
#9392 = DIRECTION('center_axis',(-1.,0.,0.)) ;
#9393 = DIRECTION('ref_axis',(0.,0.,-1.)) ;
#9394 = DIRECTION('',(0.,-1.,0.)) ;
#9395 = DIRECTION('',(0.,0.,-1.)) ;
#9396 = DIRECTION('center_axis',(0.,0.,1.)) ;
#9397 = DIRECTION('ref_axis',(-1.,0.,0.)) ;
#9398 = DIRECTION('',(-1.,0.,0.)) ;
#9399 = DIRECTION('center_axis',(0.,1.,0.)) ;
#9400 = DIRECTION('ref_axis',(1.,0.,0.)) ;
#9401 = DIRECTION('',(0.,-1.,0.)) ;
#9402 = DIRECTION('',(0.,-1.,0.)) ;
#9403 = DIRECTION('center_axis',(-1.,0.,0.)) ;
#9404 = DIRECTION('ref_axis',(0.,0.,-1.)) ;
#9405 = DIRECTION('',(0.,0.,-1.)) ;
#9406 = DIRECTION('',(0.,-1.,0.)) ;
#9407 = DIRECTION('center_axis',(0.,0.,-1.)) ;
#9408 = DIRECTION('ref_axis',(1.,0.,0.)) ;
#9409 = DIRECTION('',(1.,0.,0.)) ;
#9410 = DIRECTION('',(0.,-1.,0.)) ;
#9411 = DIRECTION('center_axis',(1.,0.,0.)) ;
#9412 = DIRECTION('ref_axis',(0.,0.,1.)) ;
#9413 = DIRECTION('',(0.,0.,1.)) ;
#9414 = DIRECTION('',(0.,-1.,0.)) ;
#9415 = DIRECTION('',(0.,-1.,0.)) ;
#9416 = DIRECTION('',(0.,-1.,0.)) ;
#9417 = DIRECTION('',(0.,-1.,0.)) ;
#9418 = DIRECTION('',(0.,-1.,0.)) ;
#9419 = DIRECTION('',(0.,-1.,0.)) ;
#9420 = DIRECTION('',(0.,-1.,0.)) ;
#9421 = DIRECTION('',(0.,-1.,0.)) ;
#9422 = DIRECTION('',(0.,-1.,0.)) ;
#9423 = DIRECTION('',(0.,-1.,0.)) ;
#9424 = DIRECTION('',(0.,-1.,0.)) ;
#9425 = DIRECTION('center_axis',(1.,0.,0.)) ;
#9426 = DIRECTION('ref_axis',(0.,0.,1.)) ;
#9427 = DIRECTION('',(0.,-1.,0.)) ;
#9428 = DIRECTION('',(0.,0.,1.)) ;
#9429 = DIRECTION('center_axis',(0.,0.,-1.)) ;
#9430 = DIRECTION('ref_axis',(1.,0.,0.)) ;
#9431 = DIRECTION('',(0.,-1.,0.)) ;
#9432 = DIRECTION('',(1.,0.,0.)) ;
#9433 = DIRECTION('center_axis',(-1.,0.,0.)) ;
#9434 = DIRECTION('ref_axis',(0.,0.,-1.)) ;
#9435 = DIRECTION('',(0.,0.,-1.)) ;
#9436 = DIRECTION('center_axis',(0.,1.,0.)) ;
#9437 = DIRECTION('ref_axis',(1.,0.,0.)) ;
#9438 = DIRECTION('',(0.,-1.,0.)) ;
#9439 = DIRECTION('',(0.,-1.,0.)) ;
#9440 = DIRECTION('',(0.,-1.,0.)) ;
#9441 = DIRECTION('',(0.,-1.,0.)) ;
#9442 = DIRECTION('center_axis',(0.0750566132645402,0.,0.997179274155484)) ;
#9443 = DIRECTION('ref_axis',(-0.997179274155484,0.,0.0750566132645402)) ;
#9444 = DIRECTION('',(-0.997179274155484,0.,0.0750566132645402)) ;
#9445 = DIRECTION('',(0.,-1.,0.)) ;
#9446 = DIRECTION('',(0.,-1.,0.)) ;
#9447 = DIRECTION('',(0.,-1.,0.)) ;
#9448 = DIRECTION('',(0.,-1.,0.)) ;
#9449 = DIRECTION('',(0.,-1.,0.)) ;
#9450 = DIRECTION('',(0.,-1.,0.)) ;
#9451 = DIRECTION('',(0.,-1.,0.)) ;
#9452 = DIRECTION('',(0.,-1.,0.)) ;
#9453 = DIRECTION('',(0.,-1.,0.)) ;
#9454 = DIRECTION('',(0.,-1.,0.)) ;
#9455 = DIRECTION('',(0.,-1.,0.)) ;
#9456 = DIRECTION('',(0.,-1.,0.)) ;
#9457 = DIRECTION('',(0.,-1.,0.)) ;
#9458 = DIRECTION('',(0.,-1.,0.)) ;
#9459 = DIRECTION('',(0.,-1.,0.)) ;
#9460 = DIRECTION('',(0.,-1.,0.)) ;
#9461 = DIRECTION('',(0.,-1.,0.)) ;
#9462 = DIRECTION('',(0.,-1.,0.)) ;
#9463 = DIRECTION('',(0.,-1.,0.)) ;
#9464 = DIRECTION('',(0.,-1.,0.)) ;
#9465 = DIRECTION('',(0.,-1.,0.)) ;
#9466 = DIRECTION('',(0.,-1.,0.)) ;
#9467 = DIRECTION('',(0.,-1.,0.)) ;
#9468 = DIRECTION('',(0.,-1.,0.)) ;
#9469 = DIRECTION('',(0.,-1.,0.)) ;
#9470 = DIRECTION('',(0.,-1.,0.)) ;
#9471 = DIRECTION('',(0.,-1.,0.)) ;
#9472 = DIRECTION('',(0.,-1.,0.)) ;
#9473 = DIRECTION('',(0.,-1.,0.)) ;
#9474 = DIRECTION('',(0.,-1.,0.)) ;
#9475 = DIRECTION('center_axis',(-0.0870991451328652,0.,-0.996199648121361)) ;
#9476 = DIRECTION('ref_axis',(0.996199648121361,0.,-0.0870991451328652)) ;
#9477 = DIRECTION('',(0.,-1.,0.)) ;
#9478 = DIRECTION('',(0.996199648121361,0.,-0.0870991451328652)) ;
#9479 = DIRECTION('center_axis',(0.,1.,0.)) ;
#9480 = DIRECTION('ref_axis',(1.,0.,0.)) ;
#9481 = DIRECTION('center_axis',(0.,0.,-1.)) ;
#9482 = DIRECTION('ref_axis',(1.,0.,0.)) ;
#9483 = DIRECTION('',(0.,-1.,0.)) ;
#9484 = DIRECTION('',(1.,0.,0.)) ;
#9485 = DIRECTION('',(0.,-1.,0.)) ;
#9486 = DIRECTION('center_axis',(1.,0.,0.)) ;
#9487 = DIRECTION('ref_axis',(0.,0.,1.)) ;
#9488 = DIRECTION('',(0.,0.,1.)) ;
#9489 = DIRECTION('',(0.,-1.,0.)) ;
#9490 = DIRECTION('center_axis',(0.,0.,1.)) ;
#9491 = DIRECTION('ref_axis',(-1.,0.,0.)) ;
#9492 = DIRECTION('',(-1.,0.,0.)) ;
#9493 = DIRECTION('',(0.,-1.,0.)) ;
#9494 = DIRECTION('center_axis',(-1.,0.,0.)) ;
#9495 = DIRECTION('ref_axis',(0.,0.,-1.)) ;
#9496 = DIRECTION('',(0.,0.,-1.)) ;
#9497 = DIRECTION('',(0.,-1.,0.)) ;
#9498 = DIRECTION('center_axis',(0.944683590425841,0.,0.327983100144111)) ;
#9499 = DIRECTION('ref_axis',(-0.327983100144111,0.,0.944683590425841)) ;
#9500 = DIRECTION('',(-0.327983100144111,0.,0.944683590425841)) ;
#9501 = DIRECTION('',(0.,-1.,0.)) ;
#9502 = DIRECTION('center_axis',(0.,0.,1.)) ;
#9503 = DIRECTION('ref_axis',(-1.,0.,0.)) ;
#9504 = DIRECTION('',(-1.,0.,0.)) ;
#9505 = DIRECTION('',(0.,-1.,0.)) ;
#9506 = DIRECTION('center_axis',(-0.946846702516136,0.,0.321685128556358)) ;
#9507 = DIRECTION('ref_axis',(-0.321685128556358,0.,-0.946846702516135)) ;
#9508 = DIRECTION('',(-0.321685128556358,0.,-0.946846702516135)) ;
#9509 = DIRECTION('',(0.,-1.,0.)) ;
#9510 = DIRECTION('center_axis',(1.,0.,0.)) ;
#9511 = DIRECTION('ref_axis',(0.,0.,1.)) ;
#9512 = DIRECTION('',(0.,0.,1.)) ;
#9513 = DIRECTION('',(0.,-1.,0.)) ;
#9514 = DIRECTION('center_axis',(-0.945579694085495,0.,-0.325390599331299)) ;
#9515 = DIRECTION('ref_axis',(0.325390599331299,0.,-0.945579694085495)) ;
#9516 = DIRECTION('',(0.,-1.,0.)) ;
#9517 = DIRECTION('',(0.325390599331299,0.,-0.945579694085495)) ;
#9518 = DIRECTION('',(0.,-1.,0.)) ;
#9519 = DIRECTION('',(0.,-1.,0.)) ;
#9520 = DIRECTION('center_axis',(0.948408846174048,0.,-0.317049933762509)) ;
#9521 = DIRECTION('ref_axis',(0.317049933762509,0.,0.948408846174048)) ;
#9522 = DIRECTION('',(0.,-1.,0.)) ;
#9523 = DIRECTION('',(0.317049933762509,0.,0.948408846174048)) ;
#9524 = DIRECTION('center_axis',(0.,0.,-1.)) ;
#9525 = DIRECTION('ref_axis',(1.,0.,0.)) ;
#9526 = DIRECTION('',(0.,-1.,0.)) ;
#9527 = DIRECTION('',(1.,0.,0.)) ;
#9528 = DIRECTION('center_axis',(-1.,0.,0.)) ;
#9529 = DIRECTION('ref_axis',(0.,0.,-1.)) ;
#9530 = DIRECTION('',(0.,-1.,0.)) ;
#9531 = DIRECTION('',(0.,0.,-1.)) ;
#9532 = DIRECTION('center_axis',(0.,0.,1.)) ;
#9533 = DIRECTION('ref_axis',(-1.,0.,0.)) ;
#9534 = DIRECTION('',(-1.,0.,0.)) ;
#9535 = DIRECTION('center_axis',(0.,1.,0.)) ;
#9536 = DIRECTION('ref_axis',(1.,0.,0.)) ;
#9537 = DIRECTION('center_axis',(1.,0.,0.)) ;
#9538 = DIRECTION('ref_axis',(0.,1.,0.)) ;
#9539 = DIRECTION('center_axis',(1.,0.,0.)) ;
#9540 = DIRECTION('ref_axis',(0.,0.,-1.)) ;
#9541 = DIRECTION('',(1.,0.,0.)) ;
#9542 = DIRECTION('center_axis',(1.,0.,0.)) ;
#9543 = DIRECTION('ref_axis',(0.,0.,-1.)) ;
#9544 = DIRECTION('center_axis',(-1.,0.,0.)) ;
#9545 = DIRECTION('ref_axis',(0.,0.,1.)) ;
#9546 = DIRECTION('center_axis',(-1.,0.,0.)) ;
#9547 = DIRECTION('ref_axis',(0.,1.,0.)) ;
#9548 = DIRECTION('center_axis',(1.,0.,0.)) ;
#9549 = DIRECTION('ref_axis',(0.,0.,-1.)) ;
#9550 = DIRECTION('center_axis',(1.,0.,0.)) ;
#9551 = DIRECTION('ref_axis',(0.,1.,0.)) ;
#9552 = DIRECTION('center_axis',(1.,0.,0.)) ;
#9553 = DIRECTION('ref_axis',(0.,-0.707106781186547,0.707106781186548)) ;
#9554 = DIRECTION('',(-0.707106781186548,-0.347335095474414,0.615920718479075)) ;
#9555 = DIRECTION('center_axis',(-1.,0.,0.)) ;
#9556 = DIRECTION('ref_axis',(0.,0.,-1.)) ;
#9557 = DIRECTION('center_axis',(-1.,0.,0.)) ;
#9558 = DIRECTION('ref_axis',(0.,0.,-1.)) ;
#9559 = DIRECTION('',(0.707106781186545,0.615920718479078,-0.347335095474413)) ;
#9560 = DIRECTION('center_axis',(1.,0.,0.)) ;
#9561 = DIRECTION('ref_axis',(0.,0.,-1.)) ;
#9562 = DIRECTION('center_axis',(1.,0.,0.)) ;
#9563 = DIRECTION('ref_axis',(0.,0.,-1.)) ;
#9564 = DIRECTION('center_axis',(1.,0.,0.)) ;
#9565 = DIRECTION('ref_axis',(0.,-1.,2.86509167645202E-16)) ;
#9566 = DIRECTION('center_axis',(1.,0.,0.)) ;
#9567 = DIRECTION('ref_axis',(0.,-1.,2.86509167645202E-16)) ;
#9568 = DIRECTION('center_axis',(1.,0.,0.)) ;
#9569 = DIRECTION('ref_axis',(0.,-1.,2.86509167645202E-16)) ;
#9570 = DIRECTION('center_axis',(1.,0.,0.)) ;
#9571 = DIRECTION('ref_axis',(0.,-1.,2.86509167645202E-16)) ;
#9572 = DIRECTION('center_axis',(0.,-1.,0.)) ;
#9573 = DIRECTION('ref_axis',(0.,0.,1.)) ;
#9574 = DIRECTION('center_axis',(-1.,0.,0.)) ;
#9575 = DIRECTION('ref_axis',(0.,-1.,2.86509167645202E-16)) ;
#9576 = DIRECTION('center_axis',(-1.,0.,0.)) ;
#9577 = DIRECTION('ref_axis',(0.,-1.,2.86509167645202E-16)) ;
#9578 = DIRECTION('center_axis',(1.,0.,0.)) ;
#9579 = DIRECTION('ref_axis',(0.,-1.,2.86509167645202E-16)) ;
#9580 = DIRECTION('center_axis',(-1.,0.,0.)) ;
#9581 = DIRECTION('ref_axis',(0.,0.,-1.)) ;
#9582 = DIRECTION('',(-1.,0.,0.)) ;
#9583 = DIRECTION('center_axis',(-1.,0.,0.)) ;
#9584 = DIRECTION('ref_axis',(0.,0.,-1.)) ;
#9585 = DIRECTION('center_axis',(1.,0.,0.)) ;
#9586 = DIRECTION('ref_axis',(0.,0.707106781186547,0.707106781186548)) ;
#9587 = DIRECTION('',(-0.707106781186548,0.615920718479075,0.347335095474414)) ;
#9588 = DIRECTION('center_axis',(-1.,0.,0.)) ;
#9589 = DIRECTION('ref_axis',(0.,0.,-1.)) ;
#9590 = DIRECTION('center_axis',(-1.,0.,0.)) ;
#9591 = DIRECTION('ref_axis',(0.,0.,-1.)) ;
#9592 = DIRECTION('',(0.707106781186548,-0.347335095474414,-0.615920718479075)) ;
#9593 = DIRECTION('center_axis',(1.,0.,0.)) ;
#9594 = DIRECTION('ref_axis',(0.,0.,-1.)) ;
#9595 = DIRECTION('center_axis',(-1.,0.,0.)) ;
#9596 = DIRECTION('ref_axis',(0.,0.,-1.)) ;
#9597 = DIRECTION('',(-1.,0.,0.)) ;
#9598 = DIRECTION('center_axis',(-1.,0.,0.)) ;
#9599 = DIRECTION('ref_axis',(0.,0.,-1.)) ;
#9600 = DIRECTION('center_axis',(1.,0.,0.)) ;
#9601 = DIRECTION('ref_axis',(0.,0.707106781186548,-0.707106781186547)) ;
#9602 = DIRECTION('',(-0.70710678118654,0.347335095474421,-0.615920718479079)) ;
#9603 = DIRECTION('center_axis',(-1.,0.,0.)) ;
#9604 = DIRECTION('ref_axis',(0.,0.,-1.)) ;
#9605 = DIRECTION('center_axis',(-1.,0.,0.)) ;
#9606 = DIRECTION('ref_axis',(0.,0.,-1.)) ;
#9607 = DIRECTION('',(0.707106781186546,-0.615920718479074,0.347335095474418)) ;
#9608 = DIRECTION('center_axis',(1.,0.,0.)) ;
#9609 = DIRECTION('ref_axis',(0.,0.,-1.)) ;
#9610 = DIRECTION('center_axis',(-1.,0.,0.)) ;
#9611 = DIRECTION('ref_axis',(0.,0.,-1.)) ;
#9612 = DIRECTION('',(-1.,0.,0.)) ;
#9613 = DIRECTION('center_axis',(-1.,0.,0.)) ;
#9614 = DIRECTION('ref_axis',(0.,0.,-1.)) ;
#9615 = DIRECTION('center_axis',(1.,0.,0.)) ;
#9616 = DIRECTION('ref_axis',(0.,-0.707106781186547,-0.707106781186548)) ;
#9617 = DIRECTION('',(-0.707106781186544,-0.615920718479077,-0.347335095474417)) ;
#9618 = DIRECTION('center_axis',(-1.,0.,0.)) ;
#9619 = DIRECTION('ref_axis',(0.,0.,-1.)) ;
#9620 = DIRECTION('center_axis',(-1.,0.,0.)) ;
#9621 = DIRECTION('ref_axis',(0.,0.,-1.)) ;
#9622 = DIRECTION('',(0.707106781186544,0.347335095474417,0.615920718479077)) ;
#9623 = DIRECTION('center_axis',(1.,0.,0.)) ;
#9624 = DIRECTION('ref_axis',(0.,0.,-1.)) ;
#9625 = DIRECTION('center_axis',(-1.,0.,0.)) ;
#9626 = DIRECTION('ref_axis',(0.,0.,-1.)) ;
#9627 = DIRECTION('',(-1.,0.,0.)) ;
#9628 = DIRECTION('center_axis',(-1.,0.,0.)) ;
#9629 = DIRECTION('ref_axis',(0.,0.,-1.)) ;
#9630 = DIRECTION('center_axis',(1.,0.,0.)) ;
#9631 = DIRECTION('ref_axis',(0.,0.,-1.)) ;
#9632 = DIRECTION('center_axis',(1.,0.,0.)) ;
#9633 = DIRECTION('ref_axis',(0.,0.,-1.)) ;
#9634 = DIRECTION('center_axis',(1.,0.,0.)) ;
#9635 = DIRECTION('ref_axis',(0.,0.,-1.)) ;
#9636 = DIRECTION('center_axis',(1.,0.,0.)) ;
#9637 = DIRECTION('ref_axis',(0.,0.,-1.)) ;
#9638 = DIRECTION('center_axis',(1.,0.,0.)) ;
#9639 = DIRECTION('ref_axis',(0.,0.,-1.)) ;
#9640 = DIRECTION('center_axis',(1.,0.,0.)) ;
#9641 = DIRECTION('ref_axis',(0.,0.,-1.)) ;
#9642 = DIRECTION('center_axis',(1.,0.,0.)) ;
#9643 = DIRECTION('ref_axis',(0.,0.,-1.)) ;
#9644 = DIRECTION('center_axis',(1.,0.,0.)) ;
#9645 = DIRECTION('ref_axis',(0.,0.,-1.)) ;
#9646 = DIRECTION('center_axis',(-1.,0.,0.)) ;
#9647 = DIRECTION('ref_axis',(0.,0.,-1.)) ;
#9648 = DIRECTION('',(-1.,0.,0.)) ;
#9649 = DIRECTION('center_axis',(1.,0.,0.)) ;
#9650 = DIRECTION('ref_axis',(0.,0.,-1.)) ;
#9651 = DIRECTION('center_axis',(-1.,0.,0.)) ;
#9652 = DIRECTION('ref_axis',(0.,0.,-1.)) ;
#9653 = DIRECTION('',(-1.,0.,0.)) ;
#9654 = DIRECTION('center_axis',(1.,0.,0.)) ;
#9655 = DIRECTION('ref_axis',(0.,0.,-1.)) ;
#9656 = DIRECTION('center_axis',(-1.,0.,0.)) ;
#9657 = DIRECTION('ref_axis',(0.,0.,-1.)) ;
#9658 = DIRECTION('',(-1.,0.,0.)) ;
#9659 = DIRECTION('center_axis',(1.,0.,0.)) ;
#9660 = DIRECTION('ref_axis',(0.,0.,-1.)) ;
#9661 = DIRECTION('center_axis',(-1.,0.,0.)) ;
#9662 = DIRECTION('ref_axis',(0.,0.,-1.)) ;
#9663 = DIRECTION('',(-1.,0.,0.)) ;
#9664 = DIRECTION('center_axis',(1.,0.,0.)) ;
#9665 = DIRECTION('ref_axis',(0.,0.,-1.)) ;
#9666 = DIRECTION('center_axis',(1.,0.,0.)) ;
#9667 = DIRECTION('ref_axis',(0.,0.,-1.)) ;
#9668 = DIRECTION('',(1.,0.,0.)) ;
#9669 = DIRECTION('center_axis',(1.,0.,0.)) ;
#9670 = DIRECTION('ref_axis',(0.,0.,-1.)) ;
#9671 = DIRECTION('',(-1.,0.,0.)) ;
#9672 = DIRECTION('center_axis',(-1.,0.,0.)) ;
#9673 = DIRECTION('ref_axis',(0.,0.,-1.)) ;
#9674 = DIRECTION('center_axis',(1.,0.,0.)) ;
#9675 = DIRECTION('ref_axis',(0.,0.,-1.)) ;
#9676 = DIRECTION('',(1.,0.,0.)) ;
#9677 = DIRECTION('center_axis',(1.,0.,0.)) ;
#9678 = DIRECTION('ref_axis',(0.,0.,-1.)) ;
#9679 = DIRECTION('',(-1.,0.,0.)) ;
#9680 = DIRECTION('center_axis',(-1.,0.,0.)) ;
#9681 = DIRECTION('ref_axis',(0.,0.,-1.)) ;
#9682 = DIRECTION('center_axis',(1.,0.,0.)) ;
#9683 = DIRECTION('ref_axis',(0.,0.707106781186548,0.707106781186547)) ;
#9684 = DIRECTION('',(-1.,0.,0.)) ;
#9685 = DIRECTION('center_axis',(-1.,0.,0.)) ;
#9686 = DIRECTION('ref_axis',(0.,0.,-1.)) ;
#9687 = DIRECTION('',(1.,0.,0.)) ;
#9688 = DIRECTION('center_axis',(1.,0.,0.)) ;
#9689 = DIRECTION('ref_axis',(0.,0.,-1.)) ;
#9690 = DIRECTION('center_axis',(1.,0.,0.)) ;
#9691 = DIRECTION('ref_axis',(0.,-0.707106781186547,0.707106781186548)) ;
#9692 = DIRECTION('',(-1.,0.,0.)) ;
#9693 = DIRECTION('center_axis',(-1.,0.,0.)) ;
#9694 = DIRECTION('ref_axis',(0.,0.,-1.)) ;
#9695 = DIRECTION('',(1.,0.,0.)) ;
#9696 = DIRECTION('center_axis',(1.,0.,0.)) ;
#9697 = DIRECTION('ref_axis',(0.,0.,-1.)) ;
#9698 = DIRECTION('center_axis',(1.,0.,0.)) ;
#9699 = DIRECTION('ref_axis',(0.,0.,-1.)) ;
#9700 = DIRECTION('center_axis',(1.,0.,0.)) ;
#9701 = DIRECTION('ref_axis',(0.,0.,-1.)) ;
#9702 = DIRECTION('center_axis',(1.,0.,0.)) ;
#9703 = DIRECTION('ref_axis',(0.,0.,-1.)) ;
#9704 = DIRECTION('center_axis',(1.,0.,0.)) ;
#9705 = DIRECTION('ref_axis',(0.,0.,-1.)) ;
#9706 = DIRECTION('center_axis',(1.,0.,0.)) ;
#9707 = DIRECTION('ref_axis',(0.,0.,-1.)) ;
#9708 = DIRECTION('center_axis',(1.,0.,0.)) ;
#9709 = DIRECTION('ref_axis',(0.,0.,-1.)) ;
#9710 = DIRECTION('center_axis',(1.,0.,0.)) ;
#9711 = DIRECTION('ref_axis',(0.,1.,0.)) ;
#9712 = DIRECTION('center_axis',(1.,0.,0.)) ;
#9713 = DIRECTION('ref_axis',(0.,0.,-1.)) ;
#9714 = DIRECTION('center_axis',(1.,0.,0.)) ;
#9715 = DIRECTION('ref_axis',(0.,1.,0.)) ;
#9716 = DIRECTION('center_axis',(1.,0.,0.)) ;
#9717 = DIRECTION('ref_axis',(0.,0.,-1.)) ;
#9718 = DIRECTION('center_axis',(1.,0.,0.)) ;
#9719 = DIRECTION('ref_axis',(0.,-1.,-1.22464679914735E-16)) ;
#9720 = DIRECTION('center_axis',(1.,0.,0.)) ;
#9721 = DIRECTION('ref_axis',(0.,0.,-1.)) ;
#9722 = DIRECTION('center_axis',(1.,0.,0.)) ;
#9723 = DIRECTION('ref_axis',(0.,1.,0.)) ;
#9724 = DIRECTION('center_axis',(1.,0.,0.)) ;
#9725 = DIRECTION('ref_axis',(0.,0.,-1.)) ;
#9726 = DIRECTION('center_axis',(1.,0.,0.)) ;
#9727 = DIRECTION('ref_axis',(0.,0.,-1.)) ;
#9728 = DIRECTION('center_axis',(1.,0.,0.)) ;
#9729 = DIRECTION('ref_axis',(0.,0.,-1.)) ;
#9730 = DIRECTION('center_axis',(1.,0.,0.)) ;
#9731 = DIRECTION('ref_axis',(0.,1.,0.)) ;
#9732 = DIRECTION('',(-1.,0.,0.)) ;
#9733 = DIRECTION('center_axis',(-1.,0.,0.)) ;
#9734 = DIRECTION('ref_axis',(0.,0.,1.)) ;
#9735 = DIRECTION('center_axis',(1.,0.,0.)) ;
#9736 = DIRECTION('ref_axis',(0.,0.,-1.)) ;
#9737 = DIRECTION('center_axis',(1.,0.,0.)) ;
#9738 = DIRECTION('ref_axis',(0.,1.,0.)) ;
#9739 = DIRECTION('center_axis',(1.,0.,0.)) ;
#9740 = DIRECTION('ref_axis',(0.,1.,0.)) ;
#9741 = DIRECTION('',(1.,0.,0.)) ;
#9742 = DIRECTION('center_axis',(1.,0.,0.)) ;
#9743 = DIRECTION('ref_axis',(0.,0.,-1.)) ;
#9744 = DIRECTION('center_axis',(1.,0.,0.)) ;
#9745 = DIRECTION('ref_axis',(0.,0.,-1.)) ;
#9746 = DIRECTION('center_axis',(-1.,0.,0.)) ;
#9747 = DIRECTION('ref_axis',(0.,1.,0.)) ;
#9748 = DIRECTION('center_axis',(1.,0.,0.)) ;
#9749 = DIRECTION('ref_axis',(0.,1.,0.)) ;
#9750 = DIRECTION('center_axis',(1.,0.,0.)) ;
#9751 = DIRECTION('ref_axis',(0.,0.,-1.)) ;
#9752 = DIRECTION('',(-1.,0.,0.)) ;
#9753 = DIRECTION('center_axis',(-1.,0.,0.)) ;
#9754 = DIRECTION('ref_axis',(0.,0.,1.)) ;
#9755 = DIRECTION('center_axis',(1.,0.,0.)) ;
#9756 = DIRECTION('ref_axis',(0.,0.,-1.)) ;
#9757 = DIRECTION('center_axis',(1.,0.,0.)) ;
#9758 = DIRECTION('ref_axis',(0.,1.,0.)) ;
#9759 = DIRECTION('center_axis',(1.,0.,0.)) ;
#9760 = DIRECTION('ref_axis',(0.,1.,0.)) ;
#9761 = DIRECTION('',(1.,0.,0.)) ;
#9762 = DIRECTION('center_axis',(1.,0.,0.)) ;
#9763 = DIRECTION('ref_axis',(0.,0.,-1.)) ;
#9764 = DIRECTION('center_axis',(1.,0.,0.)) ;
#9765 = DIRECTION('ref_axis',(0.,0.,-1.)) ;
#9766 = DIRECTION('center_axis',(-1.,0.,0.)) ;
#9767 = DIRECTION('ref_axis',(0.,1.,0.)) ;
#9768 = DIRECTION('center_axis',(1.,0.,0.)) ;
#9769 = DIRECTION('ref_axis',(0.,1.,0.)) ;
#9770 = DIRECTION('center_axis',(1.,0.,0.)) ;
#9771 = DIRECTION('ref_axis',(0.,0.,-1.)) ;
#9772 = DIRECTION('',(-1.,0.,0.)) ;
#9773 = DIRECTION('center_axis',(-1.,0.,0.)) ;
#9774 = DIRECTION('ref_axis',(0.,0.,1.)) ;
#9775 = DIRECTION('center_axis',(1.,0.,0.)) ;
#9776 = DIRECTION('ref_axis',(0.,1.,0.)) ;
#9777 = DIRECTION('',(-1.,0.,0.)) ;
#9778 = DIRECTION('center_axis',(1.,0.,0.)) ;
#9779 = DIRECTION('ref_axis',(0.,0.,-1.)) ;
#9780 = DIRECTION('center_axis',(-1.,0.,0.)) ;
#9781 = DIRECTION('ref_axis',(0.,0.,1.)) ;
#9782 = DIRECTION('center_axis',(1.,0.,0.)) ;
#9783 = DIRECTION('ref_axis',(0.,0.,-1.)) ;
#9784 = DIRECTION('center_axis',(1.,0.,0.)) ;
#9785 = DIRECTION('ref_axis',(0.,1.,0.)) ;
#9786 = DIRECTION('center_axis',(1.,0.,0.)) ;
#9787 = DIRECTION('ref_axis',(0.,0.,-1.)) ;
#9788 = DIRECTION('',(-0.707106781186548,0.707106781186548,8.65956056235493E-17)) ;
#9789 = DIRECTION('center_axis',(1.,0.,0.)) ;
#9790 = DIRECTION('ref_axis',(0.,1.,0.)) ;
#9791 = DIRECTION('center_axis',(1.,0.,0.)) ;
#9792 = DIRECTION('ref_axis',(0.,0.,-1.)) ;
#9793 = DIRECTION('',(-1.,0.,0.)) ;
#9794 = DIRECTION('center_axis',(-1.,0.,0.)) ;
#9795 = DIRECTION('ref_axis',(0.,1.,0.)) ;
#9796 = DIRECTION('',(-0.707106781186548,-0.707106781186548,-8.65956056235493E-17)) ;
#9797 = DIRECTION('center_axis',(-1.,0.,0.)) ;
#9798 = DIRECTION('ref_axis',(0.,1.,0.)) ;
#9799 = DIRECTION('center_axis',(1.,0.,0.)) ;
#9800 = DIRECTION('ref_axis',(0.,0.,-1.)) ;
#9801 = DIRECTION('',(-0.707106781186548,-0.707106781186548,-8.65956056235493E-17)) ;
#9802 = DIRECTION('center_axis',(1.,0.,0.)) ;
#9803 = DIRECTION('ref_axis',(0.,0.,-1.)) ;
#9804 = DIRECTION('center_axis',(1.,0.,0.)) ;
#9805 = DIRECTION('ref_axis',(0.,1.,0.)) ;
#9806 = DIRECTION('',(-1.,0.,0.)) ;
#9807 = DIRECTION('axis',(0.,0.,1.)) ;
#9808 = DIRECTION('refdir',(1.,0.,0.)) ;
#9809 = DIRECTION('center_axis',(0.,0.707106781186547,-0.707106781186548)) ;
#9810 = DIRECTION('ref_axis',(0.,0.707106781186548,0.707106781186547)) ;
#9811 = DIRECTION('',(1.,0.,0.)) ;
#9812 = DIRECTION('',(0.,-0.707106781186548,-0.707106781186547)) ;
#9813 = DIRECTION('',(-1.,0.,0.)) ;
#9814 = DIRECTION('',(0.,0.707106781186548,0.707106781186547)) ;
#9815 = DIRECTION('center_axis',(1.,0.,0.)) ;
#9816 = DIRECTION('ref_axis',(0.,0.,-1.)) ;
#9817 = DIRECTION('center_axis',(-1.,0.,0.)) ;
#9818 = DIRECTION('ref_axis',(0.,1.,0.)) ;
#9819 = DIRECTION('center_axis',(1.,0.,0.)) ;
#9820 = DIRECTION('ref_axis',(0.,1.,0.)) ;
#9821 = DIRECTION('',(0.,-0.707106781186547,-0.707106781186548)) ;
#9822 = DIRECTION('center_axis',(0.,-0.707106781186548,0.707106781186547)) ;
#9823 = DIRECTION('ref_axis',(0.,-0.707106781186547,-0.707106781186548)) ;
#9824 = DIRECTION('',(-1.,0.,0.)) ;
#9825 = DIRECTION('',(1.,0.,0.)) ;
#9826 = DIRECTION('',(0.,0.707106781186547,0.707106781186548)) ;
#9827 = DIRECTION('center_axis',(1.,0.,0.)) ;
#9828 = DIRECTION('ref_axis',(0.,0.,-1.)) ;
#9829 = DIRECTION('center_axis',(1.,0.,0.)) ;
#9830 = DIRECTION('ref_axis',(0.,1.,0.)) ;
#9831 = DIRECTION('center_axis',(-1.,0.,0.)) ;
#9832 = DIRECTION('ref_axis',(0.,1.,0.)) ;
#9833 = DIRECTION('center_axis',(0.,0.707106781186549,0.707106781186546)) ;
#9834 = DIRECTION('ref_axis',(0.,-0.707106781186546,0.707106781186549)) ;
#9835 = DIRECTION('',(1.,0.,0.)) ;
#9836 = DIRECTION('',(0.,0.707106781186546,-0.707106781186549)) ;
#9837 = DIRECTION('',(-1.,0.,0.)) ;
#9838 = DIRECTION('',(0.,-0.707106781186546,0.707106781186549)) ;
#9839 = DIRECTION('center_axis',(1.,0.,0.)) ;
#9840 = DIRECTION('ref_axis',(0.,0.,-1.)) ;
#9841 = DIRECTION('center_axis',(-1.,0.,0.)) ;
#9842 = DIRECTION('ref_axis',(0.,1.,0.)) ;
#9843 = DIRECTION('center_axis',(1.,0.,0.)) ;
#9844 = DIRECTION('ref_axis',(0.,1.,0.)) ;
#9845 = DIRECTION('',(0.,0.707106781186548,-0.707106781186547)) ;
#9846 = DIRECTION('center_axis',(0.,-0.707106781186547,-0.707106781186548)) ;
#9847 = DIRECTION('ref_axis',(0.,0.707106781186548,-0.707106781186547)) ;
#9848 = DIRECTION('',(-1.,0.,0.)) ;
#9849 = DIRECTION('',(1.,0.,0.)) ;
#9850 = DIRECTION('',(0.,-0.707106781186548,0.707106781186547)) ;
#9851 = DIRECTION('center_axis',(1.,0.,0.)) ;
#9852 = DIRECTION('ref_axis',(0.,0.,-1.)) ;
#9853 = DIRECTION('center_axis',(1.,0.,0.)) ;
#9854 = DIRECTION('ref_axis',(0.,1.,0.)) ;
#9855 = DIRECTION('center_axis',(-1.,0.,0.)) ;
#9856 = DIRECTION('ref_axis',(0.,1.,0.)) ;
#9857 = DIRECTION('center_axis',(0.,-0.707106781186546,0.707106781186549)) ;
#9858 = DIRECTION('ref_axis',(0.,-0.707106781186549,-0.707106781186546)) ;
#9859 = DIRECTION('',(1.,0.,0.)) ;
#9860 = DIRECTION('',(0.,0.707106781186549,0.707106781186546)) ;
#9861 = DIRECTION('',(-1.,0.,0.)) ;
#9862 = DIRECTION('',(0.,-0.707106781186549,-0.707106781186546)) ;
#9863 = DIRECTION('center_axis',(1.,0.,0.)) ;
#9864 = DIRECTION('ref_axis',(0.,0.,-1.)) ;
#9865 = DIRECTION('center_axis',(-1.,0.,0.)) ;
#9866 = DIRECTION('ref_axis',(0.,1.,0.)) ;
#9867 = DIRECTION('center_axis',(1.,0.,0.)) ;
#9868 = DIRECTION('ref_axis',(0.,1.,0.)) ;
#9869 = DIRECTION('',(0.,0.707106781186546,0.707106781186549)) ;
#9870 = DIRECTION('center_axis',(0.,0.707106781186549,-0.707106781186546)) ;
#9871 = DIRECTION('ref_axis',(0.,0.707106781186546,0.707106781186549)) ;
#9872 = DIRECTION('',(-1.,0.,0.)) ;
#9873 = DIRECTION('',(1.,0.,0.)) ;
#9874 = DIRECTION('',(0.,-0.707106781186546,-0.707106781186549)) ;
#9875 = DIRECTION('center_axis',(1.,0.,0.)) ;
#9876 = DIRECTION('ref_axis',(0.,0.,-1.)) ;
#9877 = DIRECTION('center_axis',(1.,0.,0.)) ;
#9878 = DIRECTION('ref_axis',(0.,1.,0.)) ;
#9879 = DIRECTION('center_axis',(-1.,0.,0.)) ;
#9880 = DIRECTION('ref_axis',(0.,1.,0.)) ;
#9881 = DIRECTION('center_axis',(0.,-0.707106781186548,-0.707106781186547)) ;
#9882 = DIRECTION('ref_axis',(0.,0.707106781186547,-0.707106781186548)) ;
#9883 = DIRECTION('',(1.,0.,0.)) ;
#9884 = DIRECTION('',(0.,-0.707106781186547,0.707106781186548)) ;
#9885 = DIRECTION('',(-1.,0.,0.)) ;
#9886 = DIRECTION('',(0.,0.707106781186547,-0.707106781186548)) ;
#9887 = DIRECTION('center_axis',(1.,0.,0.)) ;
#9888 = DIRECTION('ref_axis',(0.,0.,-1.)) ;
#9889 = DIRECTION('center_axis',(-1.,0.,0.)) ;
#9890 = DIRECTION('ref_axis',(0.,1.,0.)) ;
#9891 = DIRECTION('center_axis',(1.,0.,0.)) ;
#9892 = DIRECTION('ref_axis',(0.,1.,0.)) ;
#9893 = DIRECTION('',(0.,-0.707106781186546,0.707106781186549)) ;
#9894 = DIRECTION('center_axis',(0.,0.707106781186549,0.707106781186546)) ;
#9895 = DIRECTION('ref_axis',(0.,-0.707106781186546,0.707106781186549)) ;
#9896 = DIRECTION('',(-1.,0.,0.)) ;
#9897 = DIRECTION('',(1.,0.,0.)) ;
#9898 = DIRECTION('',(0.,0.707106781186546,-0.707106781186549)) ;
#9899 = DIRECTION('center_axis',(1.,0.,0.)) ;
#9900 = DIRECTION('ref_axis',(0.,0.,-1.)) ;
#9901 = DIRECTION('center_axis',(1.,0.,0.)) ;
#9902 = DIRECTION('ref_axis',(0.,1.,0.)) ;
#9903 = DIRECTION('center_axis',(-1.,0.,0.)) ;
#9904 = DIRECTION('ref_axis',(0.,1.,0.)) ;
#9905 = DIRECTION('center_axis',(1.,0.,0.)) ;
#9906 = DIRECTION('ref_axis',(0.,1.,0.)) ;
#9907 = DIRECTION('center_axis',(1.,0.,0.)) ;
#9908 = DIRECTION('ref_axis',(0.,0.,-1.)) ;
#9909 = DIRECTION('',(-1.,0.,0.)) ;
#9910 = DIRECTION('center_axis',(1.,0.,0.)) ;
#9911 = DIRECTION('ref_axis',(0.,0.,-1.)) ;
#9912 = DIRECTION('center_axis',(-1.,0.,0.)) ;
#9913 = DIRECTION('ref_axis',(0.,0.,1.)) ;
#9914 = DIRECTION('center_axis',(1.,0.,0.)) ;
#9915 = DIRECTION('ref_axis',(0.,0.,-1.)) ;
#9916 = DIRECTION('center_axis',(1.,0.,0.)) ;
#9917 = DIRECTION('ref_axis',(0.,1.,0.)) ;
#9918 = DIRECTION('center_axis',(1.,0.,0.)) ;
#9919 = DIRECTION('ref_axis',(0.,0.,-1.)) ;
#9920 = DIRECTION('',(-1.,0.,0.)) ;
#9921 = DIRECTION('center_axis',(1.,0.,0.)) ;
#9922 = DIRECTION('ref_axis',(0.,0.,-1.)) ;
#9923 = DIRECTION('axis',(0.,0.,1.)) ;
#9924 = DIRECTION('refdir',(1.,0.,0.)) ;
#9925 = DIRECTION('center_axis',(0.,0.,1.)) ;
#9926 = DIRECTION('ref_axis',(1.,0.,0.)) ;
#9927 = DIRECTION('center_axis',(0.,-1.,0.)) ;
#9928 = DIRECTION('ref_axis',(-1.,0.,0.)) ;
#9929 = DIRECTION('axis',(0.,0.,1.)) ;
#9930 = DIRECTION('refdir',(1.,0.,0.)) ;
#9931 = DIRECTION('center_axis',(-1.,0.,0.)) ;
#9932 = DIRECTION('ref_axis',(0.,0.,-1.)) ;
#9933 = DIRECTION('',(1.,0.,0.)) ;
#9934 = DIRECTION('center_axis',(1.,0.,0.)) ;
#9935 = DIRECTION('ref_axis',(0.,0.,-1.)) ;
#9936 = DIRECTION('center_axis',(-1.,0.,0.)) ;
#9937 = DIRECTION('ref_axis',(0.,0.,-1.)) ;
#9938 = DIRECTION('',(1.,0.,0.)) ;
#9939 = DIRECTION('center_axis',(-1.,0.,0.)) ;
#9940 = DIRECTION('ref_axis',(0.,0.,-1.)) ;
#9941 = DIRECTION('',(1.,0.,0.)) ;
#9942 = DIRECTION('center_axis',(-1.,0.,0.)) ;
#9943 = DIRECTION('ref_axis',(0.,0.,-1.)) ;
#9944 = DIRECTION('',(1.,0.,0.)) ;
#9945 = DIRECTION('center_axis',(-1.,0.,0.)) ;
#9946 = DIRECTION('ref_axis',(0.,0.,-1.)) ;
#9947 = DIRECTION('',(1.,0.,0.)) ;
#9948 = DIRECTION('center_axis',(-1.,0.,0.)) ;
#9949 = DIRECTION('ref_axis',(0.,0.,-1.)) ;
#9950 = DIRECTION('',(1.,0.,0.)) ;
#9951 = DIRECTION('center_axis',(-1.,0.,0.)) ;
#9952 = DIRECTION('ref_axis',(0.,0.,-1.)) ;
#9953 = DIRECTION('',(1.,0.,0.)) ;
#9954 = DIRECTION('center_axis',(-1.,0.,0.)) ;
#9955 = DIRECTION('ref_axis',(0.,0.,-1.)) ;
#9956 = DIRECTION('',(1.,0.,0.)) ;
#9957 = DIRECTION('center_axis',(-1.,0.,0.)) ;
#9958 = DIRECTION('ref_axis',(0.,0.,-1.)) ;
#9959 = DIRECTION('',(1.,0.,0.)) ;
#9960 = DIRECTION('center_axis',(-1.,0.,0.)) ;
#9961 = DIRECTION('ref_axis',(0.,0.,-1.)) ;
#9962 = DIRECTION('',(1.,0.,0.)) ;
#9963 = DIRECTION('center_axis',(-1.,0.,0.)) ;
#9964 = DIRECTION('ref_axis',(0.,0.,-1.)) ;
#9965 = DIRECTION('',(1.,0.,0.)) ;
#9966 = DIRECTION('center_axis',(-1.,0.,0.)) ;
#9967 = DIRECTION('ref_axis',(0.,0.,-1.)) ;
#9968 = DIRECTION('',(1.,0.,0.)) ;
#9969 = DIRECTION('center_axis',(-1.,0.,0.)) ;
#9970 = DIRECTION('ref_axis',(0.,0.,-1.)) ;
#9971 = DIRECTION('',(1.,0.,0.)) ;
#9972 = DIRECTION('center_axis',(-1.,0.,0.)) ;
#9973 = DIRECTION('ref_axis',(0.,0.,-1.)) ;
#9974 = DIRECTION('',(1.,0.,0.)) ;
#9975 = DIRECTION('center_axis',(-1.,0.,0.)) ;
#9976 = DIRECTION('ref_axis',(0.,0.,-1.)) ;
#9977 = DIRECTION('center_axis',(-1.,0.,0.)) ;
#9978 = DIRECTION('ref_axis',(0.,0.912319398217867,-0.409479322598088)) ;
#9979 = DIRECTION('',(-1.,0.,0.)) ;
#9980 = DIRECTION('center_axis',(-1.,0.,0.)) ;
#9981 = DIRECTION('ref_axis',(0.,-7.70839515651023E-14,-1.)) ;
#9982 = DIRECTION('center_axis',(-1.,0.,0.)) ;
#9983 = DIRECTION('ref_axis',(0.,-7.70839515651023E-14,-1.)) ;
#9984 = DIRECTION('',(-1.,0.,0.)) ;
#9985 = DIRECTION('center_axis',(-1.,0.,0.)) ;
#9986 = DIRECTION('ref_axis',(0.,-7.70839515651023E-14,-1.)) ;
#9987 = DIRECTION('',(-1.,0.,0.)) ;
#9988 = DIRECTION('center_axis',(-1.,0.,0.)) ;
#9989 = DIRECTION('ref_axis',(0.,-7.70839515651023E-14,-1.)) ;
#9990 = DIRECTION('',(-1.,0.,0.)) ;
#9991 = DIRECTION('center_axis',(-1.,0.,0.)) ;
#9992 = DIRECTION('ref_axis',(0.,-7.70839515651023E-14,-1.)) ;
#9993 = DIRECTION('',(-1.,0.,0.)) ;
#9994 = DIRECTION('center_axis',(-1.,0.,0.)) ;
#9995 = DIRECTION('ref_axis',(0.,-7.70839515651023E-14,-1.)) ;
#9996 = DIRECTION('',(-1.,0.,0.)) ;
#9997 = DIRECTION('center_axis',(-1.,0.,0.)) ;
#9998 = DIRECTION('ref_axis',(0.,-7.70839515651023E-14,-1.)) ;
#9999 = DIRECTION('',(-1.,0.,0.)) ;
#10000 = DIRECTION('center_axis',(-1.,0.,0.)) ;
#10001 = DIRECTION('ref_axis',(0.,-7.70839515651023E-14,-1.)) ;
#10002 = DIRECTION('',(-1.,0.,0.)) ;
#10003 = DIRECTION('center_axis',(-1.,0.,0.)) ;
#10004 = DIRECTION('ref_axis',(0.,-7.70839515651023E-14,-1.)) ;
#10005 = DIRECTION('',(-1.,0.,0.)) ;
#10006 = DIRECTION('center_axis',(-1.,0.,0.)) ;
#10007 = DIRECTION('ref_axis',(0.,-7.70839515651023E-14,-1.)) ;
#10008 = DIRECTION('',(-1.,0.,0.)) ;
#10009 = DIRECTION('center_axis',(-1.,0.,0.)) ;
#10010 = DIRECTION('ref_axis',(0.,-7.70839515651023E-14,-1.)) ;
#10011 = DIRECTION('',(-1.,0.,0.)) ;
#10012 = DIRECTION('center_axis',(-1.,0.,0.)) ;
#10013 = DIRECTION('ref_axis',(0.,-7.70839515651023E-14,-1.)) ;
#10014 = DIRECTION('',(-1.,0.,0.)) ;
#10015 = DIRECTION('center_axis',(-1.,0.,0.)) ;
#10016 = DIRECTION('ref_axis',(0.,-7.70839515651023E-14,-1.)) ;
#10017 = DIRECTION('',(-1.,0.,0.)) ;
#10018 = DIRECTION('center_axis',(1.,0.,0.)) ;
#10019 = DIRECTION('ref_axis',(0.,0.,-1.)) ;
#10020 = DIRECTION('center_axis',(-1.,0.,0.)) ;
#10021 = DIRECTION('ref_axis',(0.,0.,-1.)) ;
#10022 = DIRECTION('center_axis',(1.,0.,0.)) ;
#10023 = DIRECTION('ref_axis',(0.,0.,-1.)) ;
#10024 = DIRECTION('center_axis',(1.,0.,0.)) ;
#10025 = DIRECTION('ref_axis',(0.,0.,-1.)) ;
#10026 = DIRECTION('center_axis',(1.,0.,0.)) ;
#10027 = DIRECTION('ref_axis',(0.,-7.70839515651023E-14,-1.)) ;
#10028 = DIRECTION('center_axis',(1.,0.,0.)) ;
#10029 = DIRECTION('ref_axis',(0.,0.,-1.)) ;
#10030 = DIRECTION('center_axis',(-1.,0.,0.)) ;
#10031 = DIRECTION('ref_axis',(0.,-7.70839515651023E-14,-1.)) ;
#10032 = DIRECTION('center_axis',(1.,0.,0.)) ;
#10033 = DIRECTION('ref_axis',(0.,0.,-1.)) ;
#10034 = DIRECTION('center_axis',(0.,-1.,0.)) ;
#10035 = DIRECTION('ref_axis',(0.,0.,1.)) ;
#10036 = DIRECTION('center_axis',(-1.,0.,0.)) ;
#10037 = DIRECTION('ref_axis',(0.,0.,-1.)) ;
#10038 = DIRECTION('center_axis',(-1.,0.,0.)) ;
#10039 = DIRECTION('ref_axis',(0.,0.33373437595002,0.942667155633021)) ;
#10040 = DIRECTION('center_axis',(-1.,0.,0.)) ;
#10041 = DIRECTION('ref_axis',(0.,0.,-1.)) ;
#10042 = DIRECTION('center_axis',(1.,0.,0.)) ;
#10043 = DIRECTION('ref_axis',(0.,0.,-1.)) ;
#10044 = DIRECTION('center_axis',(1.,0.,0.)) ;
#10045 = DIRECTION('ref_axis',(0.,0.,-1.)) ;
#10046 = DIRECTION('center_axis',(1.,0.,0.)) ;
#10047 = DIRECTION('ref_axis',(0.,0.,-1.)) ;
#10048 = DIRECTION('',(-0.707106781186548,8.65956056235493E-17,-0.707106781186548)) ;
#10049 = DIRECTION('center_axis',(1.,0.,0.)) ;
#10050 = DIRECTION('ref_axis',(0.,0.,-1.)) ;
#10051 = DIRECTION('center_axis',(1.,0.,0.)) ;
#10052 = DIRECTION('ref_axis',(0.,0.,-1.)) ;
#10053 = DIRECTION('center_axis',(0.,-0.588540350318076,0.808467844782634)) ;
#10054 = DIRECTION('ref_axis',(0.,0.808467844782634,0.588540350318076)) ;
#10055 = DIRECTION('',(-1.,0.,0.)) ;
#10056 = DIRECTION('',(0.,0.808467844782634,0.588540350318076)) ;
#10057 = DIRECTION('',(-1.,0.,0.)) ;
#10058 = DIRECTION('center_axis',(-1.,0.,0.)) ;
#10059 = DIRECTION('ref_axis',(0.,-0.17364817766693,0.984807753012208)) ;
#10060 = DIRECTION('center_axis',(-1.,0.,0.)) ;
#10061 = DIRECTION('ref_axis',(0.,0.,-1.)) ;
#10062 = DIRECTION('',(0.,-0.961003922853656,0.276534736081898)) ;
#10063 = DIRECTION('center_axis',(0.,-0.276534736081898,-0.961003922853656)) ;
#10064 = DIRECTION('ref_axis',(0.,-0.961003922853656,0.276534736081898)) ;
#10065 = DIRECTION('',(1.,0.,0.)) ;
#10066 = DIRECTION('center_axis',(1.,0.,0.)) ;
#10067 = DIRECTION('ref_axis',(0.,0.,-1.)) ;
#10068 = DIRECTION('center_axis',(1.,0.,0.)) ;
#10069 = DIRECTION('ref_axis',(0.,0.,-1.)) ;
#10070 = DIRECTION('',(-1.,0.,0.)) ;
#10071 = DIRECTION('center_axis',(-1.,0.,0.)) ;
#10072 = DIRECTION('ref_axis',(0.,0.,-1.)) ;
#10073 = DIRECTION('',(1.,0.,0.)) ;
#10074 = DIRECTION('center_axis',(1.,0.,0.)) ;
#10075 = DIRECTION('ref_axis',(0.,0.,-1.)) ;
#10076 = DIRECTION('',(-1.,0.,0.)) ;
#10077 = DIRECTION('center_axis',(-1.,0.,0.)) ;
#10078 = DIRECTION('ref_axis',(0.,0.,-1.)) ;
#10079 = DIRECTION('',(1.,0.,0.)) ;
#10080 = DIRECTION('center_axis',(1.,0.,0.)) ;
#10081 = DIRECTION('ref_axis',(0.,0.,-1.)) ;
#10082 = DIRECTION('',(-1.,0.,0.)) ;
#10083 = DIRECTION('center_axis',(-1.,0.,0.)) ;
#10084 = DIRECTION('ref_axis',(0.,0.,-1.)) ;
#10085 = DIRECTION('',(1.,0.,0.)) ;
#10086 = DIRECTION('center_axis',(1.,0.,0.)) ;
#10087 = DIRECTION('ref_axis',(0.,0.,-1.)) ;
#10088 = DIRECTION('',(-1.,0.,0.)) ;
#10089 = DIRECTION('center_axis',(-1.,0.,0.)) ;
#10090 = DIRECTION('ref_axis',(0.,0.,-1.)) ;
#10091 = DIRECTION('',(1.,0.,0.)) ;
#10092 = DIRECTION('center_axis',(1.,0.,0.)) ;
#10093 = DIRECTION('ref_axis',(0.,0.,-1.)) ;
#10094 = DIRECTION('',(-1.,0.,0.)) ;
#10095 = DIRECTION('center_axis',(-1.,0.,0.)) ;
#10096 = DIRECTION('ref_axis',(0.,0.,-1.)) ;
#10097 = DIRECTION('',(1.,0.,0.)) ;
#10098 = DIRECTION('center_axis',(1.,0.,0.)) ;
#10099 = DIRECTION('ref_axis',(0.,0.,-1.)) ;
#10100 = DIRECTION('',(-1.,0.,0.)) ;
#10101 = DIRECTION('center_axis',(-1.,0.,0.)) ;
#10102 = DIRECTION('ref_axis',(0.,0.,-1.)) ;
#10103 = DIRECTION('',(1.,0.,0.)) ;
#10104 = DIRECTION('center_axis',(1.,0.,0.)) ;
#10105 = DIRECTION('ref_axis',(0.,0.,-1.)) ;
#10106 = DIRECTION('',(-1.,0.,0.)) ;
#10107 = DIRECTION('center_axis',(-1.,0.,0.)) ;
#10108 = DIRECTION('ref_axis',(0.,0.,-1.)) ;
#10109 = DIRECTION('',(1.,0.,0.)) ;
#10110 = DIRECTION('center_axis',(1.,0.,0.)) ;
#10111 = DIRECTION('ref_axis',(0.,0.,-1.)) ;
#10112 = DIRECTION('',(-1.,0.,0.)) ;
#10113 = DIRECTION('center_axis',(-1.,0.,0.)) ;
#10114 = DIRECTION('ref_axis',(0.,0.,-1.)) ;
#10115 = DIRECTION('',(1.,0.,0.)) ;
#10116 = DIRECTION('center_axis',(1.,0.,0.)) ;
#10117 = DIRECTION('ref_axis',(0.,0.,-1.)) ;
#10118 = DIRECTION('',(-1.,0.,0.)) ;
#10119 = DIRECTION('center_axis',(-1.,0.,0.)) ;
#10120 = DIRECTION('ref_axis',(0.,0.,-1.)) ;
#10121 = DIRECTION('',(1.,0.,0.)) ;
#10122 = DIRECTION('center_axis',(1.,0.,0.)) ;
#10123 = DIRECTION('ref_axis',(0.,0.,-1.)) ;
#10124 = DIRECTION('',(-1.,0.,0.)) ;
#10125 = DIRECTION('center_axis',(-1.,0.,0.)) ;
#10126 = DIRECTION('ref_axis',(0.,0.,-1.)) ;
#10127 = DIRECTION('',(1.,0.,0.)) ;
#10128 = DIRECTION('center_axis',(1.,0.,0.)) ;
#10129 = DIRECTION('ref_axis',(0.,0.,-1.)) ;
#10130 = DIRECTION('',(-1.,0.,0.)) ;
#10131 = DIRECTION('center_axis',(-1.,0.,0.)) ;
#10132 = DIRECTION('ref_axis',(0.,0.,-1.)) ;
#10133 = DIRECTION('',(1.,0.,0.)) ;
#10134 = DIRECTION('center_axis',(1.,0.,0.)) ;
#10135 = DIRECTION('ref_axis',(0.,0.,-1.)) ;
#10136 = DIRECTION('',(-1.,0.,0.)) ;
#10137 = DIRECTION('center_axis',(-1.,0.,0.)) ;
#10138 = DIRECTION('ref_axis',(0.,0.,-1.)) ;
#10139 = DIRECTION('',(1.,0.,0.)) ;
#10140 = DIRECTION('center_axis',(1.,0.,0.)) ;
#10141 = DIRECTION('ref_axis',(0.,0.,-1.)) ;
#10142 = DIRECTION('',(-1.,0.,0.)) ;
#10143 = DIRECTION('center_axis',(-1.,0.,0.)) ;
#10144 = DIRECTION('ref_axis',(0.,0.,-1.)) ;
#10145 = DIRECTION('',(1.,0.,0.)) ;
#10146 = DIRECTION('center_axis',(1.,0.,0.)) ;
#10147 = DIRECTION('ref_axis',(0.,0.,-1.)) ;
#10148 = DIRECTION('',(-1.,0.,0.)) ;
#10149 = DIRECTION('center_axis',(-1.,0.,0.)) ;
#10150 = DIRECTION('ref_axis',(0.,0.,-1.)) ;
#10151 = DIRECTION('',(1.,0.,0.)) ;
#10152 = DIRECTION('center_axis',(1.,0.,0.)) ;
#10153 = DIRECTION('ref_axis',(0.,0.,-1.)) ;
#10154 = DIRECTION('',(-1.,0.,0.)) ;
#10155 = DIRECTION('center_axis',(-1.,0.,0.)) ;
#10156 = DIRECTION('ref_axis',(0.,0.,-1.)) ;
#10157 = DIRECTION('',(1.,0.,0.)) ;
#10158 = DIRECTION('center_axis',(1.,0.,0.)) ;
#10159 = DIRECTION('ref_axis',(0.,0.,-1.)) ;
#10160 = DIRECTION('',(-1.,0.,0.)) ;
#10161 = DIRECTION('center_axis',(-1.,0.,0.)) ;
#10162 = DIRECTION('ref_axis',(0.,0.,-1.)) ;
#10163 = DIRECTION('',(1.,0.,0.)) ;
#10164 = DIRECTION('center_axis',(1.,0.,0.)) ;
#10165 = DIRECTION('ref_axis',(0.,0.,-1.)) ;
#10166 = DIRECTION('',(-1.,0.,0.)) ;
#10167 = DIRECTION('center_axis',(-1.,0.,0.)) ;
#10168 = DIRECTION('ref_axis',(0.,0.,-1.)) ;
#10169 = DIRECTION('',(1.,0.,0.)) ;
#10170 = DIRECTION('center_axis',(1.,0.,0.)) ;
#10171 = DIRECTION('ref_axis',(0.,0.,-1.)) ;
#10172 = DIRECTION('',(-1.,0.,0.)) ;
#10173 = DIRECTION('center_axis',(-1.,0.,0.)) ;
#10174 = DIRECTION('ref_axis',(0.,0.,-1.)) ;
#10175 = DIRECTION('',(1.,0.,0.)) ;
#10176 = DIRECTION('center_axis',(1.,0.,0.)) ;
#10177 = DIRECTION('ref_axis',(0.,0.,-1.)) ;
#10178 = DIRECTION('',(-1.,0.,0.)) ;
#10179 = DIRECTION('center_axis',(-1.,0.,0.)) ;
#10180 = DIRECTION('ref_axis',(0.,0.,-1.)) ;
#10181 = DIRECTION('',(1.,0.,0.)) ;
#10182 = DIRECTION('center_axis',(1.,0.,0.)) ;
#10183 = DIRECTION('ref_axis',(0.,0.,-1.)) ;
#10184 = DIRECTION('',(-1.,0.,0.)) ;
#10185 = DIRECTION('center_axis',(-1.,0.,0.)) ;
#10186 = DIRECTION('ref_axis',(0.,0.,-1.)) ;
#10187 = DIRECTION('',(1.,0.,0.)) ;
#10188 = DIRECTION('center_axis',(1.,0.,0.)) ;
#10189 = DIRECTION('ref_axis',(0.,0.,-1.)) ;
#10190 = DIRECTION('',(-1.,0.,0.)) ;
#10191 = DIRECTION('center_axis',(-1.,0.,0.)) ;
#10192 = DIRECTION('ref_axis',(0.,0.,-1.)) ;
#10193 = DIRECTION('',(1.,0.,0.)) ;
#10194 = DIRECTION('center_axis',(1.,0.,0.)) ;
#10195 = DIRECTION('ref_axis',(0.,0.,-1.)) ;
#10196 = DIRECTION('',(-1.,0.,0.)) ;
#10197 = DIRECTION('center_axis',(-1.,0.,0.)) ;
#10198 = DIRECTION('ref_axis',(0.,0.,-1.)) ;
#10199 = DIRECTION('',(1.,0.,0.)) ;
#10200 = DIRECTION('center_axis',(1.,0.,0.)) ;
#10201 = DIRECTION('ref_axis',(0.,0.,-1.)) ;
#10202 = DIRECTION('',(-1.,0.,0.)) ;
#10203 = DIRECTION('center_axis',(-1.,0.,0.)) ;
#10204 = DIRECTION('ref_axis',(0.,0.,-1.)) ;
#10205 = DIRECTION('',(1.,0.,0.)) ;
#10206 = DIRECTION('center_axis',(1.,0.,0.)) ;
#10207 = DIRECTION('ref_axis',(0.,0.,-1.)) ;
#10208 = DIRECTION('',(-1.,0.,0.)) ;
#10209 = DIRECTION('center_axis',(-1.,0.,0.)) ;
#10210 = DIRECTION('ref_axis',(0.,0.,-1.)) ;
#10211 = DIRECTION('',(1.,0.,0.)) ;
#10212 = DIRECTION('center_axis',(1.,0.,0.)) ;
#10213 = DIRECTION('ref_axis',(0.,0.,-1.)) ;
#10214 = DIRECTION('',(-1.,0.,0.)) ;
#10215 = DIRECTION('center_axis',(-1.,0.,0.)) ;
#10216 = DIRECTION('ref_axis',(0.,0.,-1.)) ;
#10217 = DIRECTION('',(1.,0.,0.)) ;
#10218 = DIRECTION('center_axis',(1.,0.,0.)) ;
#10219 = DIRECTION('ref_axis',(0.,0.,-1.)) ;
#10220 = DIRECTION('',(-1.,0.,0.)) ;
#10221 = DIRECTION('center_axis',(-1.,0.,0.)) ;
#10222 = DIRECTION('ref_axis',(0.,0.,-1.)) ;
#10223 = DIRECTION('',(1.,0.,0.)) ;
#10224 = DIRECTION('center_axis',(1.,0.,0.)) ;
#10225 = DIRECTION('ref_axis',(0.,0.,-1.)) ;
#10226 = DIRECTION('',(-1.,0.,0.)) ;
#10227 = DIRECTION('center_axis',(-1.,0.,0.)) ;
#10228 = DIRECTION('ref_axis',(0.,0.,-1.)) ;
#10229 = DIRECTION('',(1.,0.,0.)) ;
#10230 = DIRECTION('center_axis',(1.,0.,0.)) ;
#10231 = DIRECTION('ref_axis',(0.,0.,-1.)) ;
#10232 = DIRECTION('',(-1.,0.,0.)) ;
#10233 = DIRECTION('center_axis',(-1.,0.,0.)) ;
#10234 = DIRECTION('ref_axis',(0.,0.,-1.)) ;
#10235 = DIRECTION('',(-1.,0.,0.)) ;
#10236 = DIRECTION('center_axis',(-1.,0.,0.)) ;
#10237 = DIRECTION('ref_axis',(0.,0.,-1.)) ;
#10238 = DIRECTION('center_axis',(-1.,0.,0.)) ;
#10239 = DIRECTION('ref_axis',(0.,0.,-1.)) ;
#10240 = DIRECTION('',(1.,0.,0.)) ;
#10241 = DIRECTION('center_axis',(1.,0.,0.)) ;
#10242 = DIRECTION('ref_axis',(0.,0.,-1.)) ;
#10243 = DIRECTION('',(-1.,0.,0.)) ;
#10244 = DIRECTION('center_axis',(-1.,0.,0.)) ;
#10245 = DIRECTION('ref_axis',(0.,0.,-1.)) ;
#10246 = DIRECTION('',(1.,0.,0.)) ;
#10247 = DIRECTION('center_axis',(1.,0.,0.)) ;
#10248 = DIRECTION('ref_axis',(0.,0.,-1.)) ;
#10249 = DIRECTION('',(-1.,0.,0.)) ;
#10250 = DIRECTION('center_axis',(-1.,0.,0.)) ;
#10251 = DIRECTION('ref_axis',(0.,0.,-1.)) ;
#10252 = DIRECTION('',(1.,0.,0.)) ;
#10253 = DIRECTION('center_axis',(1.,0.,0.)) ;
#10254 = DIRECTION('ref_axis',(0.,0.,-1.)) ;
#10255 = DIRECTION('',(-1.,0.,0.)) ;
#10256 = DIRECTION('center_axis',(-1.,0.,0.)) ;
#10257 = DIRECTION('ref_axis',(0.,0.,-1.)) ;
#10258 = DIRECTION('',(1.,0.,0.)) ;
#10259 = DIRECTION('center_axis',(1.,0.,0.)) ;
#10260 = DIRECTION('ref_axis',(0.,0.,-1.)) ;
#10261 = DIRECTION('',(-1.,0.,0.)) ;
#10262 = DIRECTION('center_axis',(-1.,0.,0.)) ;
#10263 = DIRECTION('ref_axis',(0.,0.,-1.)) ;
#10264 = DIRECTION('',(1.,0.,0.)) ;
#10265 = DIRECTION('center_axis',(1.,0.,0.)) ;
#10266 = DIRECTION('ref_axis',(0.,0.,-1.)) ;
#10267 = DIRECTION('',(-1.,0.,0.)) ;
#10268 = DIRECTION('center_axis',(-1.,0.,0.)) ;
#10269 = DIRECTION('ref_axis',(0.,0.,-1.)) ;
#10270 = DIRECTION('',(1.,0.,0.)) ;
#10271 = DIRECTION('center_axis',(1.,0.,0.)) ;
#10272 = DIRECTION('ref_axis',(0.,0.,-1.)) ;
#10273 = DIRECTION('',(-1.,0.,0.)) ;
#10274 = DIRECTION('center_axis',(-1.,0.,0.)) ;
#10275 = DIRECTION('ref_axis',(0.,0.,-1.)) ;
#10276 = DIRECTION('',(1.,0.,0.)) ;
#10277 = DIRECTION('center_axis',(1.,0.,0.)) ;
#10278 = DIRECTION('ref_axis',(0.,0.,-1.)) ;
#10279 = DIRECTION('',(-1.,0.,0.)) ;
#10280 = DIRECTION('center_axis',(-1.,0.,0.)) ;
#10281 = DIRECTION('ref_axis',(0.,0.,-1.)) ;
#10282 = DIRECTION('',(1.,0.,0.)) ;
#10283 = DIRECTION('center_axis',(1.,0.,0.)) ;
#10284 = DIRECTION('ref_axis',(0.,0.,-1.)) ;
#10285 = DIRECTION('center_axis',(0.,-0.719988067902578,0.693986442286817)) ;
#10286 = DIRECTION('ref_axis',(0.,0.693986442286817,0.719988067902578)) ;
#10287 = DIRECTION('',(-1.,0.,0.)) ;
#10288 = DIRECTION('',(0.,0.693986442286817,0.719988067902578)) ;
#10289 = DIRECTION('center_axis',(-1.,0.,0.)) ;
#10290 = DIRECTION('ref_axis',(0.,-0.342020143325669,0.939692620785908)) ;
#10291 = DIRECTION('',(0.,-0.994423866883653,0.105456972136329)) ;
#10292 = DIRECTION('center_axis',(0.,-0.105456972136329,-0.994423866883653)) ;
#10293 = DIRECTION('ref_axis',(0.,-0.994423866883653,0.105456972136329)) ;
#10294 = DIRECTION('center_axis',(0.,-0.8295593123754,0.5584186129162)) ;
#10295 = DIRECTION('ref_axis',(0.,0.5584186129162,0.8295593123754)) ;
#10296 = DIRECTION('',(-1.,0.,0.)) ;
#10297 = DIRECTION('',(0.,0.5584186129162,0.8295593123754)) ;
#10298 = DIRECTION('center_axis',(-1.,0.,0.)) ;
#10299 = DIRECTION('ref_axis',(0.,-0.5,0.866025403784438)) ;
#10300 = DIRECTION('',(0.,-0.997628744921147,-0.0688250485437991)) ;
#10301 = DIRECTION('center_axis',(0.,0.0688250485437991,-0.997628744921147)) ;
#10302 = DIRECTION('ref_axis',(0.,-0.997628744921147,-0.0688250485437991)) ;
#10303 = DIRECTION('center_axis',(0.,-0.913924816918964,0.405883516565577)) ;
#10304 = DIRECTION('ref_axis',(0.,0.405883516565577,0.913924816918964)) ;
#10305 = DIRECTION('',(-1.,0.,0.)) ;
#10306 = DIRECTION('',(0.,0.405883516565577,0.913924816918964)) ;
#10307 = DIRECTION('center_axis',(-1.,0.,0.)) ;
#10308 = DIRECTION('ref_axis',(0.,-0.64278760968654,0.766044443118978)) ;
#10309 = DIRECTION('',(0.,-0.970521178368716,-0.241015854951079)) ;
#10310 = DIRECTION('center_axis',(0.,0.241015854951079,-0.970521178368716)) ;
#10311 = DIRECTION('ref_axis',(0.,-0.970521178368716,-0.241015854951079)) ;
#10312 = DIRECTION('center_axis',(0.,-0.970521178368716,0.241015854951078)) ;
#10313 = DIRECTION('ref_axis',(0.,0.241015854951078,0.970521178368716)) ;
#10314 = DIRECTION('',(-1.,0.,0.)) ;
#10315 = DIRECTION('',(0.,0.241015854951078,0.970521178368716)) ;
#10316 = DIRECTION('center_axis',(-1.,0.,0.)) ;
#10317 = DIRECTION('ref_axis',(0.,-0.766044443118978,0.642787609686539)) ;
#10318 = DIRECTION('',(0.,-0.913924816918963,-0.405883516565577)) ;
#10319 = DIRECTION('center_axis',(0.,0.405883516565577,-0.913924816918963)) ;
#10320 = DIRECTION('ref_axis',(0.,-0.913924816918963,-0.405883516565577)) ;
#10321 = DIRECTION('center_axis',(0.,-0.997628744921148,0.0688250485437987)) ;
#10322 = DIRECTION('ref_axis',(0.,0.0688250485437987,0.997628744921147)) ;
#10323 = DIRECTION('',(-1.,0.,0.)) ;
#10324 = DIRECTION('',(0.,0.0688250485437987,0.997628744921147)) ;
#10325 = DIRECTION('center_axis',(-1.,0.,0.)) ;
#10326 = DIRECTION('ref_axis',(0.,-0.866025403784439,0.5)) ;
#10327 = DIRECTION('',(0.,-0.8295593123754,-0.5584186129162)) ;
#10328 = DIRECTION('center_axis',(0.,0.5584186129162,-0.8295593123754)) ;
#10329 = DIRECTION('ref_axis',(0.,-0.8295593123754,-0.5584186129162)) ;
#10330 = DIRECTION('center_axis',(0.,-0.994423866883653,-0.10545697213633)) ;
#10331 = DIRECTION('ref_axis',(0.,-0.10545697213633,0.994423866883653)) ;
#10332 = DIRECTION('',(-1.,0.,0.)) ;
#10333 = DIRECTION('',(0.,-0.10545697213633,0.994423866883653)) ;
#10334 = DIRECTION('center_axis',(-1.,0.,0.)) ;
#10335 = DIRECTION('ref_axis',(0.,-0.939692620785909,0.342020143325668)) ;
#10336 = DIRECTION('',(0.,-0.719988067902577,-0.693986442286818)) ;
#10337 = DIRECTION('center_axis',(0.,0.693986442286818,-0.719988067902577)) ;
#10338 = DIRECTION('ref_axis',(0.,-0.719988067902577,-0.693986442286818)) ;
#10339 = DIRECTION('center_axis',(0.,-0.961003922853655,-0.276534736081899)) ;
#10340 = DIRECTION('ref_axis',(0.,-0.276534736081899,0.961003922853655)) ;
#10341 = DIRECTION('',(-1.,0.,0.)) ;
#10342 = DIRECTION('',(0.,-0.276534736081899,0.961003922853655)) ;
#10343 = DIRECTION('center_axis',(-1.,0.,0.)) ;
#10344 = DIRECTION('ref_axis',(0.,-0.984807753012208,0.17364817766693)) ;
#10345 = DIRECTION('',(0.,-0.588540350318076,-0.808467844782634)) ;
#10346 = DIRECTION('center_axis',(0.,0.808467844782634,-0.588540350318076)) ;
#10347 = DIRECTION('ref_axis',(0.,-0.588540350318076,-0.808467844782634)) ;
#10348 = DIRECTION('center_axis',(0.,-0.898384360919199,-0.439210132004947)) ;
#10349 = DIRECTION('ref_axis',(0.,-0.439210132004947,0.898384360919199)) ;
#10350 = DIRECTION('',(-1.,0.,0.)) ;
#10351 = DIRECTION('',(0.,-0.439210132004947,0.898384360919199)) ;
#10352 = DIRECTION('center_axis',(-1.,0.,0.)) ;
#10353 = DIRECTION('ref_axis',(0.,-1.,-1.83697019872103E-16)) ;
#10354 = DIRECTION('',(0.,-0.439210132004947,-0.898384360919199)) ;
#10355 = DIRECTION('center_axis',(0.,0.898384360919199,-0.439210132004947)) ;
#10356 = DIRECTION('ref_axis',(0.,-0.439210132004947,-0.898384360919199)) ;
#10357 = DIRECTION('center_axis',(0.,-0.808467844782634,-0.588540350318076)) ;
#10358 = DIRECTION('ref_axis',(0.,-0.588540350318076,0.808467844782634)) ;
#10359 = DIRECTION('',(-1.,0.,0.)) ;
#10360 = DIRECTION('',(0.,-0.588540350318076,0.808467844782634)) ;
#10361 = DIRECTION('center_axis',(-1.,0.,0.)) ;
#10362 = DIRECTION('ref_axis',(0.,-0.984807753012208,-0.17364817766693)) ;
#10363 = DIRECTION('',(0.,-0.276534736081898,-0.961003922853656)) ;
#10364 = DIRECTION('center_axis',(0.,0.961003922853656,-0.276534736081898)) ;
#10365 = DIRECTION('ref_axis',(0.,-0.276534736081898,-0.961003922853656)) ;
#10366 = DIRECTION('center_axis',(0.,-0.693986442286817,-0.719988067902578)) ;
#10367 = DIRECTION('ref_axis',(0.,-0.719988067902578,0.693986442286817)) ;
#10368 = DIRECTION('',(-1.,0.,0.)) ;
#10369 = DIRECTION('',(0.,-0.719988067902578,0.693986442286817)) ;
#10370 = DIRECTION('center_axis',(-1.,0.,0.)) ;
#10371 = DIRECTION('ref_axis',(0.,-0.939692620785908,-0.342020143325669)) ;
#10372 = DIRECTION('',(0.,-0.105456972136329,-0.994423866883653)) ;
#10373 = DIRECTION('center_axis',(0.,0.994423866883653,-0.105456972136329)) ;
#10374 = DIRECTION('ref_axis',(0.,-0.105456972136329,-0.994423866883653)) ;
#10375 = DIRECTION('center_axis',(0.,-0.5584186129162,-0.8295593123754)) ;
#10376 = DIRECTION('ref_axis',(0.,-0.8295593123754,0.5584186129162)) ;
#10377 = DIRECTION('',(-1.,0.,0.)) ;
#10378 = DIRECTION('',(0.,-0.8295593123754,0.5584186129162)) ;
#10379 = DIRECTION('center_axis',(-1.,0.,0.)) ;
#10380 = DIRECTION('ref_axis',(0.,-0.866025403784438,-0.5)) ;
#10381 = DIRECTION('',(0.,0.0688250485437991,-0.997628744921147)) ;
#10382 = DIRECTION('center_axis',(0.,0.997628744921147,0.0688250485437991)) ;
#10383 = DIRECTION('ref_axis',(0.,0.0688250485437991,-0.997628744921147)) ;
#10384 = DIRECTION('center_axis',(0.,-0.405883516565577,-0.913924816918964)) ;
#10385 = DIRECTION('ref_axis',(0.,-0.913924816918964,0.405883516565577)) ;
#10386 = DIRECTION('',(-1.,0.,0.)) ;
#10387 = DIRECTION('',(0.,-0.913924816918964,0.405883516565577)) ;
#10388 = DIRECTION('center_axis',(-1.,0.,0.)) ;
#10389 = DIRECTION('ref_axis',(0.,-0.766044443118978,-0.642787609686539)) ;
#10390 = DIRECTION('',(0.,0.241015854951079,-0.970521178368716)) ;
#10391 = DIRECTION('center_axis',(0.,0.970521178368716,0.241015854951079)) ;
#10392 = DIRECTION('ref_axis',(0.,0.241015854951079,-0.970521178368716)) ;
#10393 = DIRECTION('center_axis',(0.,-0.241015854951079,-0.970521178368716)) ;
#10394 = DIRECTION('ref_axis',(0.,-0.970521178368716,0.241015854951079)) ;
#10395 = DIRECTION('',(-1.,0.,0.)) ;
#10396 = DIRECTION('',(0.,-0.970521178368716,0.241015854951079)) ;
#10397 = DIRECTION('center_axis',(-1.,0.,0.)) ;
#10398 = DIRECTION('ref_axis',(0.,-0.642787609686539,-0.766044443118978)) ;
#10399 = DIRECTION('',(0.,0.405883516565577,-0.913924816918963)) ;
#10400 = DIRECTION('center_axis',(0.,0.913924816918963,0.405883516565577)) ;
#10401 = DIRECTION('ref_axis',(0.,0.405883516565577,-0.913924816918963)) ;
#10402 = DIRECTION('center_axis',(0.,-0.0688250485437983,-0.997628744921147)) ;
#10403 = DIRECTION('ref_axis',(0.,-0.997628744921147,0.0688250485437983)) ;
#10404 = DIRECTION('',(-1.,0.,0.)) ;
#10405 = DIRECTION('',(0.,-0.997628744921147,0.0688250485437983)) ;
#10406 = DIRECTION('center_axis',(-1.,0.,0.)) ;
#10407 = DIRECTION('ref_axis',(0.,-0.5,-0.866025403784439)) ;
#10408 = DIRECTION('',(0.,0.558418612916201,-0.8295593123754)) ;
#10409 = DIRECTION('center_axis',(0.,0.8295593123754,0.558418612916201)) ;
#10410 = DIRECTION('ref_axis',(0.,0.558418612916201,-0.8295593123754)) ;
#10411 = DIRECTION('center_axis',(0.,0.10545697213633,-0.994423866883653)) ;
#10412 = DIRECTION('ref_axis',(0.,-0.994423866883653,-0.10545697213633)) ;
#10413 = DIRECTION('',(-1.,0.,0.)) ;
#10414 = DIRECTION('',(0.,-0.994423866883653,-0.10545697213633)) ;
#10415 = DIRECTION('center_axis',(-1.,0.,0.)) ;
#10416 = DIRECTION('ref_axis',(0.,-0.342020143325669,-0.939692620785909)) ;
#10417 = DIRECTION('',(0.,0.693986442286818,-0.719988067902577)) ;
#10418 = DIRECTION('center_axis',(0.,0.719988067902577,0.693986442286818)) ;
#10419 = DIRECTION('ref_axis',(0.,0.693986442286818,-0.719988067902577)) ;
#10420 = DIRECTION('center_axis',(0.,0.276534736081899,-0.961003922853656)) ;
#10421 = DIRECTION('ref_axis',(0.,-0.961003922853656,-0.276534736081899)) ;
#10422 = DIRECTION('',(-1.,0.,0.)) ;
#10423 = DIRECTION('',(0.,-0.961003922853655,-0.276534736081899)) ;
#10424 = DIRECTION('center_axis',(-1.,0.,0.)) ;
#10425 = DIRECTION('ref_axis',(0.,-0.17364817766693,-0.984807753012208)) ;
#10426 = DIRECTION('',(0.,0.808467844782634,-0.588540350318076)) ;
#10427 = DIRECTION('center_axis',(0.,0.588540350318076,0.808467844782634)) ;
#10428 = DIRECTION('ref_axis',(0.,0.808467844782634,-0.588540350318076)) ;
#10429 = DIRECTION('center_axis',(0.,0.439210132004947,-0.898384360919199)) ;
#10430 = DIRECTION('ref_axis',(0.,-0.898384360919199,-0.439210132004947)) ;
#10431 = DIRECTION('',(-1.,0.,0.)) ;
#10432 = DIRECTION('',(0.,-0.898384360919199,-0.439210132004947)) ;
#10433 = DIRECTION('center_axis',(-1.,0.,0.)) ;
#10434 = DIRECTION('ref_axis',(0.,1.22464679914735E-16,-1.)) ;
#10435 = DIRECTION('',(0.,0.898384360919199,-0.439210132004947)) ;
#10436 = DIRECTION('center_axis',(0.,0.439210132004947,0.898384360919199)) ;
#10437 = DIRECTION('ref_axis',(0.,0.898384360919199,-0.439210132004947)) ;
#10438 = DIRECTION('center_axis',(0.,0.588540350318076,-0.808467844782634)) ;
#10439 = DIRECTION('ref_axis',(0.,-0.808467844782633,-0.588540350318076)) ;
#10440 = DIRECTION('',(-1.,0.,0.)) ;
#10441 = DIRECTION('',(0.,-0.808467844782633,-0.588540350318076)) ;
#10442 = DIRECTION('center_axis',(-1.,0.,0.)) ;
#10443 = DIRECTION('ref_axis',(0.,0.173648177666931,-0.984807753012208)) ;
#10444 = DIRECTION('',(0.,0.961003922853656,-0.276534736081898)) ;
#10445 = DIRECTION('center_axis',(0.,0.276534736081898,0.961003922853656)) ;
#10446 = DIRECTION('ref_axis',(0.,0.961003922853656,-0.276534736081898)) ;
#10447 = DIRECTION('center_axis',(0.,0.719988067902577,-0.693986442286817)) ;
#10448 = DIRECTION('ref_axis',(0.,-0.693986442286817,-0.719988067902577)) ;
#10449 = DIRECTION('',(-1.,0.,0.)) ;
#10450 = DIRECTION('',(0.,-0.693986442286817,-0.719988067902577)) ;
#10451 = DIRECTION('center_axis',(-1.,0.,0.)) ;
#10452 = DIRECTION('ref_axis',(0.,0.342020143325669,-0.939692620785908)) ;
#10453 = DIRECTION('',(0.,0.994423866883653,-0.10545697213633)) ;
#10454 = DIRECTION('center_axis',(0.,0.10545697213633,0.994423866883653)) ;
#10455 = DIRECTION('ref_axis',(0.,0.994423866883653,-0.10545697213633)) ;
#10456 = DIRECTION('center_axis',(0.,0.8295593123754,-0.558418612916201)) ;
#10457 = DIRECTION('ref_axis',(0.,-0.558418612916201,-0.8295593123754)) ;
#10458 = DIRECTION('',(-1.,0.,0.)) ;
#10459 = DIRECTION('',(0.,-0.558418612916201,-0.8295593123754)) ;
#10460 = DIRECTION('center_axis',(-1.,0.,0.)) ;
#10461 = DIRECTION('ref_axis',(0.,0.5,-0.866025403784439)) ;
#10462 = DIRECTION('',(0.,0.997628744921147,0.0688250485437986)) ;
#10463 = DIRECTION('center_axis',(0.,-0.0688250485437986,0.997628744921148)) ;
#10464 = DIRECTION('ref_axis',(0.,0.997628744921147,0.0688250485437986)) ;
#10465 = DIRECTION('center_axis',(0.,0.913924816918964,-0.405883516565577)) ;
#10466 = DIRECTION('ref_axis',(0.,-0.405883516565577,-0.913924816918964)) ;
#10467 = DIRECTION('',(-1.,0.,0.)) ;
#10468 = DIRECTION('',(0.,-0.405883516565577,-0.913924816918964)) ;
#10469 = DIRECTION('center_axis',(-1.,0.,0.)) ;
#10470 = DIRECTION('ref_axis',(0.,0.642787609686539,-0.766044443118978)) ;
#10471 = DIRECTION('',(0.,0.970521178368716,0.241015854951079)) ;
#10472 = DIRECTION('center_axis',(0.,-0.241015854951079,0.970521178368716)) ;
#10473 = DIRECTION('ref_axis',(0.,0.970521178368716,0.241015854951079)) ;
#10474 = DIRECTION('center_axis',(0.,0.970521178368716,-0.241015854951079)) ;
#10475 = DIRECTION('ref_axis',(0.,-0.241015854951079,-0.970521178368716)) ;
#10476 = DIRECTION('',(-1.,0.,0.)) ;
#10477 = DIRECTION('',(0.,-0.241015854951079,-0.970521178368716)) ;
#10478 = DIRECTION('center_axis',(-1.,0.,0.)) ;
#10479 = DIRECTION('ref_axis',(0.,0.766044443118978,-0.642787609686539)) ;
#10480 = DIRECTION('',(0.,0.913924816918963,0.405883516565577)) ;
#10481 = DIRECTION('center_axis',(0.,-0.405883516565577,0.913924816918964)) ;
#10482 = DIRECTION('ref_axis',(0.,0.913924816918963,0.405883516565577)) ;
#10483 = DIRECTION('center_axis',(0.,0.997628744921147,-0.0688250485437984)) ;
#10484 = DIRECTION('ref_axis',(0.,-0.0688250485437984,-0.997628744921147)) ;
#10485 = DIRECTION('',(-1.,0.,0.)) ;
#10486 = DIRECTION('',(0.,-0.0688250485437984,-0.997628744921147)) ;
#10487 = DIRECTION('center_axis',(-1.,0.,0.)) ;
#10488 = DIRECTION('ref_axis',(0.,0.866025403784439,-0.5)) ;
#10489 = DIRECTION('',(0.,0.8295593123754,0.558418612916201)) ;
#10490 = DIRECTION('center_axis',(0.,-0.558418612916201,0.8295593123754)) ;
#10491 = DIRECTION('ref_axis',(0.,0.8295593123754,0.558418612916201)) ;
#10492 = DIRECTION('center_axis',(0.,0.994423866883653,0.10545697213633)) ;
#10493 = DIRECTION('ref_axis',(0.,0.10545697213633,-0.994423866883653)) ;
#10494 = DIRECTION('',(-1.,0.,0.)) ;
#10495 = DIRECTION('',(0.,0.10545697213633,-0.994423866883653)) ;
#10496 = DIRECTION('center_axis',(-1.,0.,0.)) ;
#10497 = DIRECTION('ref_axis',(0.,0.939692620785908,-0.342020143325669)) ;
#10498 = DIRECTION('',(0.,0.719988067902577,0.693986442286817)) ;
#10499 = DIRECTION('center_axis',(0.,-0.693986442286817,0.719988067902577)) ;
#10500 = DIRECTION('ref_axis',(0.,0.719988067902577,0.693986442286817)) ;
#10501 = DIRECTION('center_axis',(0.,0.961003922853656,0.276534736081898)) ;
#10502 = DIRECTION('ref_axis',(0.,0.276534736081898,-0.961003922853656)) ;
#10503 = DIRECTION('',(-1.,0.,0.)) ;
#10504 = DIRECTION('',(0.,0.276534736081898,-0.961003922853656)) ;
#10505 = DIRECTION('center_axis',(-1.,0.,0.)) ;
#10506 = DIRECTION('ref_axis',(0.,0.984807753012208,-0.17364817766693)) ;
#10507 = DIRECTION('',(0.,0.588540350318076,0.808467844782634)) ;
#10508 = DIRECTION('center_axis',(0.,-0.808467844782634,0.588540350318076)) ;
#10509 = DIRECTION('ref_axis',(0.,0.588540350318076,0.808467844782634)) ;
#10510 = DIRECTION('center_axis',(0.,0.898384360919199,0.439210132004947)) ;
#10511 = DIRECTION('ref_axis',(0.,0.439210132004947,-0.898384360919199)) ;
#10512 = DIRECTION('',(-1.,0.,0.)) ;
#10513 = DIRECTION('',(0.,0.439210132004947,-0.898384360919199)) ;
#10514 = DIRECTION('center_axis',(-1.,0.,0.)) ;
#10515 = DIRECTION('ref_axis',(0.,1.,6.12323399573677E-17)) ;
#10516 = DIRECTION('',(0.,0.439210132004947,0.898384360919199)) ;
#10517 = DIRECTION('center_axis',(0.,-0.898384360919199,0.439210132004947)) ;
#10518 = DIRECTION('ref_axis',(0.,0.439210132004947,0.898384360919199)) ;
#10519 = DIRECTION('center_axis',(0.,0.808467844782634,0.588540350318076)) ;
#10520 = DIRECTION('ref_axis',(0.,0.588540350318076,-0.808467844782634)) ;
#10521 = DIRECTION('',(-1.,0.,0.)) ;
#10522 = DIRECTION('',(0.,0.588540350318076,-0.808467844782634)) ;
#10523 = DIRECTION('center_axis',(-1.,0.,0.)) ;
#10524 = DIRECTION('ref_axis',(0.,0.984807753012208,0.17364817766693)) ;
#10525 = DIRECTION('',(0.,0.276534736081898,0.961003922853656)) ;
#10526 = DIRECTION('center_axis',(0.,-0.961003922853656,0.276534736081898)) ;
#10527 = DIRECTION('ref_axis',(0.,0.276534736081898,0.961003922853656)) ;
#10528 = DIRECTION('center_axis',(0.,0.693986442286817,0.719988067902577)) ;
#10529 = DIRECTION('ref_axis',(0.,0.719988067902577,-0.693986442286817)) ;
#10530 = DIRECTION('',(-1.,0.,0.)) ;
#10531 = DIRECTION('',(0.,0.719988067902577,-0.693986442286817)) ;
#10532 = DIRECTION('center_axis',(-1.,0.,0.)) ;
#10533 = DIRECTION('ref_axis',(0.,0.939692620785908,0.342020143325669)) ;
#10534 = DIRECTION('',(0.,0.10545697213633,0.994423866883653)) ;
#10535 = DIRECTION('center_axis',(0.,-0.994423866883653,0.10545697213633)) ;
#10536 = DIRECTION('ref_axis',(0.,0.10545697213633,0.994423866883653)) ;
#10537 = DIRECTION('center_axis',(0.,0.5584186129162,0.8295593123754)) ;
#10538 = DIRECTION('ref_axis',(0.,0.8295593123754,-0.5584186129162)) ;
#10539 = DIRECTION('',(-1.,0.,0.)) ;
#10540 = DIRECTION('',(0.,0.8295593123754,-0.5584186129162)) ;
#10541 = DIRECTION('center_axis',(-1.,0.,0.)) ;
#10542 = DIRECTION('ref_axis',(0.,0.866025403784439,0.5)) ;
#10543 = DIRECTION('',(0.,-0.0688250485437987,0.997628744921147)) ;
#10544 = DIRECTION('center_axis',(0.,-0.997628744921148,-0.0688250485437987)) ;
#10545 = DIRECTION('ref_axis',(0.,-0.0688250485437987,0.997628744921147)) ;
#10546 = DIRECTION('center_axis',(0.,0.405883516565577,0.913924816918964)) ;
#10547 = DIRECTION('ref_axis',(0.,0.913924816918963,-0.405883516565577)) ;
#10548 = DIRECTION('',(-1.,0.,0.)) ;
#10549 = DIRECTION('',(0.,0.913924816918963,-0.405883516565577)) ;
#10550 = DIRECTION('center_axis',(-1.,0.,0.)) ;
#10551 = DIRECTION('ref_axis',(0.,0.766044443118978,0.642787609686539)) ;
#10552 = DIRECTION('',(0.,-0.241015854951079,0.970521178368716)) ;
#10553 = DIRECTION('center_axis',(0.,-0.970521178368716,-0.241015854951079)) ;
#10554 = DIRECTION('ref_axis',(0.,-0.241015854951079,0.970521178368716)) ;
#10555 = DIRECTION('center_axis',(0.,0.241015854951079,0.970521178368716)) ;
#10556 = DIRECTION('ref_axis',(0.,0.970521178368716,-0.241015854951079)) ;
#10557 = DIRECTION('',(-1.,0.,0.)) ;
#10558 = DIRECTION('',(0.,0.970521178368716,-0.241015854951079)) ;
#10559 = DIRECTION('center_axis',(-1.,0.,0.)) ;
#10560 = DIRECTION('ref_axis',(0.,0.642787609686539,0.766044443118978)) ;
#10561 = DIRECTION('',(0.,-0.405883516565577,0.913924816918963)) ;
#10562 = DIRECTION('center_axis',(0.,-0.913924816918963,-0.405883516565577)) ;
#10563 = DIRECTION('ref_axis',(0.,-0.405883516565577,0.913924816918963)) ;
#10564 = DIRECTION('center_axis',(0.,0.0688250485437986,0.997628744921148)) ;
#10565 = DIRECTION('ref_axis',(0.,0.997628744921147,-0.0688250485437986)) ;
#10566 = DIRECTION('',(-1.,0.,0.)) ;
#10567 = DIRECTION('',(0.,0.997628744921147,-0.0688250485437986)) ;
#10568 = DIRECTION('center_axis',(-1.,0.,0.)) ;
#10569 = DIRECTION('ref_axis',(0.,0.5,0.866025403784439)) ;
#10570 = DIRECTION('',(0.,-0.558418612916201,0.8295593123754)) ;
#10571 = DIRECTION('center_axis',(0.,-0.8295593123754,-0.558418612916201)) ;
#10572 = DIRECTION('ref_axis',(0.,-0.558418612916201,0.8295593123754)) ;
#10573 = DIRECTION('center_axis',(0.,-0.10545697213633,0.994423866883653)) ;
#10574 = DIRECTION('ref_axis',(0.,0.994423866883653,0.10545697213633)) ;
#10575 = DIRECTION('',(-1.,0.,0.)) ;
#10576 = DIRECTION('',(0.,0.994423866883653,0.10545697213633)) ;
#10577 = DIRECTION('center_axis',(-1.,0.,0.)) ;
#10578 = DIRECTION('ref_axis',(0.,0.342020143325669,0.939692620785908)) ;
#10579 = DIRECTION('',(0.,-0.693986442286817,0.719988067902577)) ;
#10580 = DIRECTION('center_axis',(0.,-0.719988067902577,-0.693986442286817)) ;
#10581 = DIRECTION('ref_axis',(0.,-0.693986442286817,0.719988067902577)) ;
#10582 = DIRECTION('center_axis',(0.,-0.276534736081898,0.961003922853656)) ;
#10583 = DIRECTION('ref_axis',(0.,0.961003922853656,0.276534736081898)) ;
#10584 = DIRECTION('',(-1.,0.,0.)) ;
#10585 = DIRECTION('',(0.,0.961003922853656,0.276534736081898)) ;
#10586 = DIRECTION('center_axis',(-1.,0.,0.)) ;
#10587 = DIRECTION('ref_axis',(0.,0.17364817766693,0.984807753012208)) ;
#10588 = DIRECTION('',(0.,-0.808467844782634,0.588540350318076)) ;
#10589 = DIRECTION('center_axis',(0.,-0.588540350318076,-0.808467844782634)) ;
#10590 = DIRECTION('ref_axis',(0.,-0.808467844782634,0.588540350318076)) ;
#10591 = DIRECTION('center_axis',(0.,-0.439210132004947,0.898384360919199)) ;
#10592 = DIRECTION('ref_axis',(0.,0.898384360919199,0.439210132004947)) ;
#10593 = DIRECTION('',(-1.,0.,0.)) ;
#10594 = DIRECTION('',(0.,0.898384360919199,0.439210132004947)) ;
#10595 = DIRECTION('center_axis',(-1.,0.,0.)) ;
#10596 = DIRECTION('ref_axis',(0.,0.,1.)) ;
#10597 = DIRECTION('',(0.,-0.898384360919199,0.439210132004947)) ;
#10598 = DIRECTION('center_axis',(0.,-0.439210132004947,-0.898384360919199)) ;
#10599 = DIRECTION('ref_axis',(0.,-0.898384360919199,0.439210132004947)) ;
#10600 = DIRECTION('center_axis',(1.,0.,0.)) ;
#10601 = DIRECTION('ref_axis',(0.,0.,-1.)) ;
#10602 = DIRECTION('center_axis',(0.,-1.,0.)) ;
#10603 = DIRECTION('ref_axis',(0.,0.,1.)) ;
#10604 = DIRECTION('center_axis',(-1.,0.,0.)) ;
#10605 = DIRECTION('ref_axis',(0.,0.,-1.)) ;
#10606 = DIRECTION('center_axis',(-1.,0.,0.)) ;
#10607 = DIRECTION('ref_axis',(0.,0.,-1.)) ;
#10608 = DIRECTION('',(-0.707106781186548,-8.65956056235494E-17,0.707106781186548)) ;
#10609 = DIRECTION('center_axis',(1.,0.,0.)) ;
#10610 = DIRECTION('ref_axis',(0.,0.,-1.)) ;
#10611 = DIRECTION('center_axis',(-1.,0.,0.)) ;
#10612 = DIRECTION('ref_axis',(0.,1.,0.)) ;
#10613 = DIRECTION('center_axis',(1.,0.,0.)) ;
#10614 = DIRECTION('ref_axis',(0.,1.,0.)) ;
#10615 = DIRECTION('center_axis',(1.,0.,0.)) ;
#10616 = DIRECTION('ref_axis',(0.,0.,-1.)) ;
#10617 = DIRECTION('center_axis',(1.,0.,0.)) ;
#10618 = DIRECTION('ref_axis',(0.,0.,-1.)) ;
#10619 = DIRECTION('center_axis',(1.,0.,0.)) ;
#10620 = DIRECTION('ref_axis',(0.,0.,-1.)) ;
#10621 = DIRECTION('center_axis',(1.,0.,0.)) ;
#10622 = DIRECTION('ref_axis',(0.,0.,-1.)) ;
#10623 = DIRECTION('center_axis',(1.,0.,0.)) ;
#10624 = DIRECTION('ref_axis',(0.,0.,-1.)) ;
#10625 = DIRECTION('',(0.707106781186542,-0.707106781186553,-8.659560562355E-17)) ;
#10626 = DIRECTION('center_axis',(1.,0.,0.)) ;
#10627 = DIRECTION('ref_axis',(0.,0.,-1.)) ;
#10628 = DIRECTION('center_axis',(1.,0.,0.)) ;
#10629 = DIRECTION('ref_axis',(0.,1.,0.)) ;
#10630 = DIRECTION('',(1.,0.,0.)) ;
#10631 = DIRECTION('',(-1.,0.,0.)) ;
#10632 = DIRECTION('center_axis',(1.,0.,0.)) ;
#10633 = DIRECTION('ref_axis',(0.,1.,0.)) ;
#10634 = DIRECTION('center_axis',(1.,0.,0.)) ;
#10635 = DIRECTION('ref_axis',(0.,1.,0.)) ;
#10636 = DIRECTION('',(-1.,0.,0.)) ;
#10637 = DIRECTION('center_axis',(1.,0.,0.)) ;
#10638 = DIRECTION('ref_axis',(0.,1.,0.)) ;
#10639 = DIRECTION('',(1.,0.,0.)) ;
#10640 = DIRECTION('center_axis',(1.,0.,0.)) ;
#10641 = DIRECTION('ref_axis',(0.,1.,0.)) ;
#10642 = DIRECTION('',(1.,0.,0.)) ;
#10643 = DIRECTION('',(-1.,0.,0.)) ;
#10644 = DIRECTION('center_axis',(1.,0.,0.)) ;
#10645 = DIRECTION('ref_axis',(0.,1.,0.)) ;
#10646 = DIRECTION('center_axis',(1.,0.,0.)) ;
#10647 = DIRECTION('ref_axis',(0.,1.,0.)) ;
#10648 = DIRECTION('',(-1.,0.,0.)) ;
#10649 = DIRECTION('center_axis',(1.,0.,0.)) ;
#10650 = DIRECTION('ref_axis',(0.,1.,0.)) ;
#10651 = DIRECTION('',(1.,0.,0.)) ;
#10652 = DIRECTION('center_axis',(1.,0.,0.)) ;
#10653 = DIRECTION('ref_axis',(0.,1.,0.)) ;
#10654 = DIRECTION('',(1.,0.,0.)) ;
#10655 = DIRECTION('',(-1.,0.,0.)) ;
#10656 = DIRECTION('center_axis',(1.,0.,0.)) ;
#10657 = DIRECTION('ref_axis',(0.,1.,0.)) ;
#10658 = DIRECTION('center_axis',(1.,0.,0.)) ;
#10659 = DIRECTION('ref_axis',(0.,1.,0.)) ;
#10660 = DIRECTION('',(-1.,0.,0.)) ;
#10661 = DIRECTION('center_axis',(1.,0.,0.)) ;
#10662 = DIRECTION('ref_axis',(0.,1.,0.)) ;
#10663 = DIRECTION('',(1.,0.,0.)) ;
#10664 = DIRECTION('center_axis',(0.,-0.86602540378444,0.499999999999998)) ;
#10665 = DIRECTION('ref_axis',(0.,0.499999999999998,0.86602540378444)) ;
#10666 = DIRECTION('',(0.,0.499999999999998,0.86602540378444)) ;
#10667 = DIRECTION('',(-1.,0.,0.)) ;
#10668 = DIRECTION('',(0.,0.499999999999998,0.86602540378444)) ;
#10669 = DIRECTION('',(-1.,0.,0.)) ;
#10670 = DIRECTION('center_axis',(0.,-0.86602540378444,-0.499999999999998)) ;
#10671 = DIRECTION('ref_axis',(0.,-0.499999999999998,0.86602540378444)) ;
#10672 = DIRECTION('',(0.,-0.499999999999998,0.86602540378444)) ;
#10673 = DIRECTION('',(-1.,0.,0.)) ;
#10674 = DIRECTION('',(0.,-0.499999999999998,0.86602540378444)) ;
#10675 = DIRECTION('center_axis',(0.,0.,-1.)) ;
#10676 = DIRECTION('ref_axis',(0.,-1.,0.)) ;
#10677 = DIRECTION('',(0.,-1.,0.)) ;
#10678 = DIRECTION('',(-1.,0.,0.)) ;
#10679 = DIRECTION('',(0.,-1.,0.)) ;
#10680 = DIRECTION('center_axis',(1.,0.,0.)) ;
#10681 = DIRECTION('ref_axis',(0.,0.,-1.)) ;
#10682 = DIRECTION('center_axis',(1.,0.,0.)) ;
#10683 = DIRECTION('ref_axis',(0.,0.,-1.)) ;
#10684 = DIRECTION('center_axis',(1.,0.,0.)) ;
#10685 = DIRECTION('ref_axis',(0.,0.,-1.)) ;
#10686 = DIRECTION('',(0.,-0.499999999999998,-0.86602540378444)) ;
#10687 = DIRECTION('center_axis',(1.,0.,0.)) ;
#10688 = DIRECTION('ref_axis',(0.,0.,-1.)) ;
#10689 = DIRECTION('center_axis',(1.,0.,0.)) ;
#10690 = DIRECTION('ref_axis',(0.,0.,-1.)) ;
#10691 = DIRECTION('',(0.,0.499999999999998,-0.86602540378444)) ;
#10692 = DIRECTION('center_axis',(1.,0.,0.)) ;
#10693 = DIRECTION('ref_axis',(0.,0.,-1.)) ;
#10694 = DIRECTION('',(0.,1.,0.)) ;
#10695 = DIRECTION('center_axis',(1.,0.,0.)) ;
#10696 = DIRECTION('ref_axis',(0.,0.,-1.)) ;
#10697 = DIRECTION('',(0.,0.499999999999998,-0.86602540378444)) ;
#10698 = DIRECTION('center_axis',(1.,0.,0.)) ;
#10699 = DIRECTION('ref_axis',(0.,0.,-1.)) ;
#10700 = DIRECTION('center_axis',(1.,0.,0.)) ;
#10701 = DIRECTION('ref_axis',(0.,0.,-1.)) ;
#10702 = DIRECTION('',(0.,-0.499999999999998,-0.86602540378444)) ;
#10703 = DIRECTION('center_axis',(1.,0.,0.)) ;
#10704 = DIRECTION('ref_axis',(0.,0.,-1.)) ;
#10705 = DIRECTION('center_axis',(1.,0.,0.)) ;
#10706 = DIRECTION('ref_axis',(0.,0.,-1.)) ;
#10707 = DIRECTION('center_axis',(1.,0.,0.)) ;
#10708 = DIRECTION('ref_axis',(0.,0.,-1.)) ;
#10709 = DIRECTION('center_axis',(1.,0.,0.)) ;
#10710 = DIRECTION('ref_axis',(0.,0.,-1.)) ;
#10711 = DIRECTION('center_axis',(1.,0.,0.)) ;
#10712 = DIRECTION('ref_axis',(0.,0.,-1.)) ;
#10713 = DIRECTION('center_axis',(1.,0.,0.)) ;
#10714 = DIRECTION('ref_axis',(0.,0.,-1.)) ;
#10715 = DIRECTION('center_axis',(1.,0.,0.)) ;
#10716 = DIRECTION('ref_axis',(0.,0.,-1.)) ;
#10717 = DIRECTION('center_axis',(1.,0.,0.)) ;
#10718 = DIRECTION('ref_axis',(0.,0.,-1.)) ;
#10719 = DIRECTION('',(0.,1.,0.)) ;
#10720 = DIRECTION('center_axis',(1.,0.,0.)) ;
#10721 = DIRECTION('ref_axis',(0.,0.,-1.)) ;
#10722 = DIRECTION('center_axis',(1.,0.,0.)) ;
#10723 = DIRECTION('ref_axis',(0.,1.,0.)) ;
#10724 = DIRECTION('',(0.515038074910055,-0.857167300702112,-1.04972719113862E-16)) ;
#10725 = DIRECTION('center_axis',(0.,0.86602540378444,0.499999999999998)) ;
#10726 = DIRECTION('ref_axis',(0.,0.499999999999998,-0.86602540378444)) ;
#10727 = DIRECTION('',(-1.,0.,0.)) ;
#10728 = DIRECTION('',(-1.,0.,0.)) ;
#10729 = DIRECTION('center_axis',(0.,0.,1.)) ;
#10730 = DIRECTION('ref_axis',(0.,1.,0.)) ;
#10731 = DIRECTION('center_axis',(0.,0.86602540378444,-0.499999999999998)) ;
#10732 = DIRECTION('ref_axis',(0.,-0.499999999999998,-0.86602540378444)) ;
#10733 = DIRECTION('axis',(0.,0.,1.)) ;
#10734 = DIRECTION('refdir',(1.,0.,0.)) ;
#10735 = DIRECTION('center_axis',(-1.,0.,0.)) ;
#10736 = DIRECTION('ref_axis',(0.,0.,1.)) ;
#10737 = DIRECTION('center_axis',(1.,0.,0.)) ;
#10738 = DIRECTION('ref_axis',(0.,0.,-1.)) ;
#10739 = DIRECTION('center_axis',(1.,0.,0.)) ;
#10740 = DIRECTION('ref_axis',(0.,0.,-1.)) ;
#10741 = DIRECTION('center_axis',(1.,0.,0.)) ;
#10742 = DIRECTION('ref_axis',(0.,1.,0.)) ;
#10743 = DIRECTION('center_axis',(1.,0.,0.)) ;
#10744 = DIRECTION('ref_axis',(0.,0.,-1.)) ;
#10745 = DIRECTION('',(-1.,0.,0.)) ;
#10746 = DIRECTION('center_axis',(1.,0.,0.)) ;
#10747 = DIRECTION('ref_axis',(0.,0.,-1.)) ;
#10748 = DIRECTION('center_axis',(1.,0.,0.)) ;
#10749 = DIRECTION('ref_axis',(0.,0.,-1.)) ;
#10750 = DIRECTION('center_axis',(1.,0.,0.)) ;
#10751 = DIRECTION('ref_axis',(0.,1.,0.)) ;
#10752 = DIRECTION('',(-0.616308261658108,0.787505001007588,9.64415478796476E-17)) ;
#10753 = DIRECTION('center_axis',(1.,0.,0.)) ;
#10754 = DIRECTION('ref_axis',(0.,0.,-1.)) ;
#10755 = DIRECTION('center_axis',(1.,0.,0.)) ;
#10756 = DIRECTION('ref_axis',(0.,1.,0.)) ;
#10757 = DIRECTION('',(-1.,0.,0.)) ;
#10758 = DIRECTION('center_axis',(1.,0.,0.)) ;
#10759 = DIRECTION('ref_axis',(0.,0.,-1.)) ;
#10760 = DIRECTION('center_axis',(-1.,0.,0.)) ;
#10761 = DIRECTION('ref_axis',(0.,1.,0.)) ;
#10762 = DIRECTION('',(-0.536875492193157,-0.843661487732109,-1.03318734051502E-16)) ;
#10763 = DIRECTION('center_axis',(1.,0.,0.)) ;
#10764 = DIRECTION('ref_axis',(0.,0.,-1.)) ;
#10765 = DIRECTION('center_axis',(1.,0.,0.)) ;
#10766 = DIRECTION('ref_axis',(0.,1.,0.)) ;
#10767 = DIRECTION('',(-0.536875492193157,0.843661487732109,1.03318734051502E-16)) ;
#10768 = DIRECTION('center_axis',(1.,0.,0.)) ;
#10769 = DIRECTION('ref_axis',(0.,0.,-1.)) ;
#10770 = DIRECTION('center_axis',(1.,0.,0.)) ;
#10771 = DIRECTION('ref_axis',(0.,1.,0.)) ;
#10772 = DIRECTION('',(-1.,0.,0.)) ;
#10773 = DIRECTION('center_axis',(1.,0.,0.)) ;
#10774 = DIRECTION('ref_axis',(0.,0.,-1.)) ;
#10775 = DIRECTION('center_axis',(-1.,0.,0.)) ;
#10776 = DIRECTION('ref_axis',(0.,1.,0.)) ;
#10777 = DIRECTION('',(-0.465746432832619,-0.884918222381984,-1.08371226854726E-16)) ;
#10778 = DIRECTION('axis',(0.,0.,1.)) ;
#10779 = DIRECTION('refdir',(1.,0.,0.)) ;
#10780 = DIRECTION('center_axis',(1.,0.,0.)) ;
#10781 = DIRECTION('ref_axis',(0.,0.,-1.)) ;
#10782 = DIRECTION('center_axis',(1.,0.,0.)) ;
#10783 = DIRECTION('ref_axis',(0.,0.,-1.)) ;
#10784 = DIRECTION('',(1.,0.,0.)) ;
#10785 = DIRECTION('center_axis',(-1.,0.,0.)) ;
#10786 = DIRECTION('ref_axis',(0.,0.,-1.)) ;
#10787 = DIRECTION('center_axis',(0.,0.,-1.)) ;
#10788 = DIRECTION('ref_axis',(0.,1.,0.)) ;
#10789 = DIRECTION('',(-1.,0.,0.)) ;
#10790 = DIRECTION('',(0.,1.,0.)) ;
#10791 = DIRECTION('',(1.,0.,0.)) ;
#10792 = DIRECTION('',(0.,-1.,0.)) ;
#10793 = DIRECTION('center_axis',(0.,-1.,0.)) ;
#10794 = DIRECTION('ref_axis',(0.,0.,-1.)) ;
#10795 = DIRECTION('',(0.,0.,1.)) ;
#10796 = DIRECTION('',(0.,0.,-1.)) ;
#10797 = DIRECTION('',(1.,0.,0.)) ;
#10798 = DIRECTION('center_axis',(0.,0.,-1.)) ;
#10799 = DIRECTION('ref_axis',(0.,1.,0.)) ;
#10800 = DIRECTION('',(0.,-1.,0.)) ;
#10801 = DIRECTION('',(1.,0.,0.)) ;
#10802 = DIRECTION('',(0.,1.,0.)) ;
#10803 = DIRECTION('center_axis',(1.,0.,0.)) ;
#10804 = DIRECTION('ref_axis',(0.,0.,-1.)) ;
#10805 = DIRECTION('center_axis',(-1.,0.,0.)) ;
#10806 = DIRECTION('ref_axis',(0.,0.,-1.)) ;
#10807 = DIRECTION('',(0.,-1.,0.)) ;
#10808 = DIRECTION('',(0.,0.,-1.)) ;
#10809 = DIRECTION('',(0.,1.,0.)) ;
#10810 = DIRECTION('center_axis',(1.,0.,0.)) ;
#10811 = DIRECTION('ref_axis',(0.,0.,-1.)) ;
#10812 = DIRECTION('center_axis',(-1.,0.,0.)) ;
#10813 = DIRECTION('ref_axis',(0.,0.,-1.)) ;
#10814 = DIRECTION('center_axis',(1.,0.,0.)) ;
#10815 = DIRECTION('ref_axis',(0.,0.,-1.)) ;
#10816 = DIRECTION('center_axis',(1.,0.,0.)) ;
#10817 = DIRECTION('ref_axis',(0.,0.,-1.)) ;
#10818 = DIRECTION('',(1.,0.,0.)) ;
#10819 = DIRECTION('center_axis',(0.,0.,1.)) ;
#10820 = DIRECTION('ref_axis',(0.,-1.,0.)) ;
#10821 = DIRECTION('',(1.,0.,0.)) ;
#10822 = DIRECTION('',(0.,-1.,0.)) ;
#10823 = DIRECTION('',(1.,0.,0.)) ;
#10824 = DIRECTION('center_axis',(0.,-1.,0.)) ;
#10825 = DIRECTION('ref_axis',(0.,0.,-1.)) ;
#10826 = DIRECTION('',(0.,0.,-1.)) ;
#10827 = DIRECTION('',(1.,0.,0.)) ;
#10828 = DIRECTION('center_axis',(1.,0.,0.)) ;
#10829 = DIRECTION('ref_axis',(0.,-1.,-6.12323399573677E-17)) ;
#10830 = DIRECTION('center_axis',(-1.,0.,0.)) ;
#10831 = DIRECTION('ref_axis',(0.,0.,-1.)) ;
#10832 = DIRECTION('center_axis',(0.,0.,1.)) ;
#10833 = DIRECTION('ref_axis',(0.,-1.,0.)) ;
#10834 = DIRECTION('',(0.,-1.,0.)) ;
#10835 = DIRECTION('',(-1.,0.,0.)) ;
#10836 = DIRECTION('center_axis',(1.,0.,0.)) ;
#10837 = DIRECTION('ref_axis',(0.,-1.,1.83697019872103E-16)) ;
#10838 = DIRECTION('center_axis',(1.,0.,0.)) ;
#10839 = DIRECTION('ref_axis',(0.,0.,-1.)) ;
#10840 = DIRECTION('center_axis',(1.,0.,0.)) ;
#10841 = DIRECTION('ref_axis',(0.,0.,-1.)) ;
#10842 = DIRECTION('',(0.,0.,1.)) ;
#10843 = DIRECTION('',(1.,0.,0.)) ;
#10844 = DIRECTION('',(0.,0.,1.)) ;
#10845 = DIRECTION('',(1.,0.,0.)) ;
#10846 = DIRECTION('',(0.,0.,1.)) ;
#10847 = DIRECTION('',(1.,0.,0.)) ;
#10848 = DIRECTION('',(0.,0.,1.)) ;
#10849 = DIRECTION('',(1.,0.,0.)) ;
#10850 = DIRECTION('',(0.,0.,1.)) ;
#10851 = DIRECTION('',(1.,0.,0.)) ;
#10852 = DIRECTION('',(0.,0.,1.)) ;
#10853 = DIRECTION('',(1.,0.,0.)) ;
#10854 = DIRECTION('',(0.,0.,1.)) ;
#10855 = DIRECTION('',(1.,0.,0.)) ;
#10856 = DIRECTION('',(0.,0.,1.)) ;
#10857 = DIRECTION('',(1.,0.,0.)) ;
#10858 = DIRECTION('',(0.,0.,1.)) ;
#10859 = DIRECTION('',(1.,0.,0.)) ;
#10860 = DIRECTION('',(0.,0.,1.)) ;
#10861 = DIRECTION('',(1.,0.,0.)) ;
#10862 = DIRECTION('',(0.,0.,1.)) ;
#10863 = DIRECTION('',(1.,0.,0.)) ;
#10864 = DIRECTION('',(0.,0.,1.)) ;
#10865 = DIRECTION('',(1.,0.,0.)) ;
#10866 = DIRECTION('',(0.,0.,1.)) ;
#10867 = DIRECTION('',(1.,0.,0.)) ;
#10868 = DIRECTION('',(0.,0.,1.)) ;
#10869 = DIRECTION('',(1.,0.,0.)) ;
#10870 = DIRECTION('',(0.,0.,1.)) ;
#10871 = DIRECTION('',(1.,0.,0.)) ;
#10872 = DIRECTION('',(0.,0.,1.)) ;
#10873 = DIRECTION('',(1.,0.,0.)) ;
#10874 = DIRECTION('',(0.,0.,1.)) ;
#10875 = DIRECTION('',(1.,0.,0.)) ;
#10876 = DIRECTION('',(0.,-1.,-2.22044604925031E-16)) ;
#10877 = DIRECTION('',(1.,0.,0.)) ;
#10878 = DIRECTION('',(0.,-1.,-2.22044604925031E-16)) ;
#10879 = DIRECTION('',(1.,0.,0.)) ;
#10880 = DIRECTION('',(0.,-1.,-2.22044604925031E-16)) ;
#10881 = DIRECTION('',(1.,0.,0.)) ;
#10882 = DIRECTION('',(0.,-1.,-2.22044604925031E-16)) ;
#10883 = DIRECTION('',(1.,0.,0.)) ;
#10884 = DIRECTION('',(0.,-1.,-2.22044604925031E-16)) ;
#10885 = DIRECTION('',(1.,0.,0.)) ;
#10886 = DIRECTION('',(0.,-1.,-2.22044604925031E-16)) ;
#10887 = DIRECTION('',(1.,0.,0.)) ;
#10888 = DIRECTION('',(0.,-1.,-2.22044604925031E-16)) ;
#10889 = DIRECTION('',(1.,0.,0.)) ;
#10890 = DIRECTION('',(0.,-1.,-2.22044604925031E-16)) ;
#10891 = DIRECTION('',(1.,0.,0.)) ;
#10892 = DIRECTION('',(0.,-1.,-2.22044604925031E-16)) ;
#10893 = DIRECTION('',(1.,0.,0.)) ;
#10894 = DIRECTION('',(0.,-1.,-2.22044604925031E-16)) ;
#10895 = DIRECTION('',(1.,0.,0.)) ;
#10896 = DIRECTION('',(0.,-1.,-2.22044604925031E-16)) ;
#10897 = DIRECTION('',(1.,0.,0.)) ;
#10898 = DIRECTION('',(0.,-1.22464679914735E-16,-1.)) ;
#10899 = DIRECTION('',(1.,0.,0.)) ;
#10900 = DIRECTION('',(0.,-1.22464679914735E-16,-1.)) ;
#10901 = DIRECTION('',(1.,0.,0.)) ;
#10902 = DIRECTION('',(0.,-1.22464679914735E-16,-1.)) ;
#10903 = DIRECTION('',(1.,0.,0.)) ;
#10904 = DIRECTION('',(0.,-1.22464679914735E-16,-1.)) ;
#10905 = DIRECTION('',(1.,0.,0.)) ;
#10906 = DIRECTION('',(0.,-1.22464679914735E-16,-1.)) ;
#10907 = DIRECTION('',(1.,0.,0.)) ;
#10908 = DIRECTION('',(0.,-1.22464679914735E-16,-1.)) ;
#10909 = DIRECTION('',(1.,0.,0.)) ;
#10910 = DIRECTION('',(0.,-1.22464679914735E-16,-1.)) ;
#10911 = DIRECTION('',(1.,0.,0.)) ;
#10912 = DIRECTION('',(0.,-1.22464679914735E-16,-1.)) ;
#10913 = DIRECTION('',(1.,0.,0.)) ;
#10914 = DIRECTION('',(0.,-1.22464679914735E-16,-1.)) ;
#10915 = DIRECTION('',(1.,0.,0.)) ;
#10916 = DIRECTION('',(0.,-1.22464679914735E-16,-1.)) ;
#10917 = DIRECTION('',(1.,0.,0.)) ;
#10918 = DIRECTION('',(0.,-1.22464679914735E-16,-1.)) ;
#10919 = DIRECTION('',(1.,0.,0.)) ;
#10920 = DIRECTION('',(0.,1.,-2.22044604925031E-16)) ;
#10921 = DIRECTION('',(1.,0.,0.)) ;
#10922 = DIRECTION('',(0.,1.,-2.22044604925031E-16)) ;
#10923 = DIRECTION('',(1.,0.,0.)) ;
#10924 = DIRECTION('',(0.,1.,-2.22044604925031E-16)) ;
#10925 = DIRECTION('',(1.,0.,0.)) ;
#10926 = DIRECTION('',(0.,1.,-2.22044604925031E-16)) ;
#10927 = DIRECTION('',(1.,0.,0.)) ;
#10928 = DIRECTION('',(0.,1.,-2.22044604925031E-16)) ;
#10929 = DIRECTION('',(1.,0.,0.)) ;
#10930 = DIRECTION('',(0.,1.,-2.22044604925031E-16)) ;
#10931 = DIRECTION('',(1.,0.,0.)) ;
#10932 = DIRECTION('',(0.,1.,-2.22044604925031E-16)) ;
#10933 = DIRECTION('',(1.,0.,0.)) ;
#10934 = DIRECTION('',(0.,1.,-2.22044604925031E-16)) ;
#10935 = DIRECTION('',(1.,0.,0.)) ;
#10936 = DIRECTION('',(0.,1.,-2.22044604925031E-16)) ;
#10937 = DIRECTION('',(1.,0.,0.)) ;
#10938 = DIRECTION('',(0.,1.,-2.22044604925031E-16)) ;
#10939 = DIRECTION('',(1.,0.,0.)) ;
#10940 = DIRECTION('',(0.,1.,-2.22044604925031E-16)) ;
#10941 = DIRECTION('',(1.,0.,0.)) ;
#10942 = DIRECTION('',(0.,-1.,-2.22044604925031E-16)) ;
#10943 = DIRECTION('',(1.,0.,0.)) ;
#10944 = DIRECTION('',(0.,-1.22464679914735E-16,-1.)) ;
#10945 = DIRECTION('',(1.,0.,0.)) ;
#10946 = DIRECTION('',(0.,1.,-2.22044604925031E-16)) ;
#10947 = DIRECTION('',(1.,0.,0.)) ;
#10948 = DIRECTION('',(1.22464679914735E-16,0.,-1.)) ;
#10949 = DIRECTION('',(-1.,0.,-1.22464679914735E-16)) ;
#10950 = DIRECTION('',(1.22464679914735E-16,0.,-1.)) ;
#10951 = DIRECTION('',(-1.,0.,-1.22464679914735E-16)) ;
#10952 = CARTESIAN_POINT('',(0.,0.,0.)) ;
#10953 = CARTESIAN_POINT('',(0.,0.,0.)) ;
#10954 = CARTESIAN_POINT('Origin',(119.75,25.5,25.5)) ;
#10955 = CARTESIAN_POINT('',(120.,25.5,30.05)) ;
#10956 = CARTESIAN_POINT('Origin',(120.,25.5,25.5)) ;
#10957 = CARTESIAN_POINT('',(119.5,25.5,29.55)) ;
#10958 = CARTESIAN_POINT('',(119.75,25.5,29.8)) ;
#10959 = CARTESIAN_POINT('Origin',(119.5,25.5,25.5)) ;
#10960 = CARTESIAN_POINT('Origin',(120.,25.5,25.5)) ;
#10961 = CARTESIAN_POINT('',(104.,25.5,29.55)) ;
#10962 = CARTESIAN_POINT('',(120.,25.5,29.55)) ;
#10963 = CARTESIAN_POINT('',(104.,21.45,25.5)) ;
#10964 = CARTESIAN_POINT('Origin',(104.,25.5,25.5)) ;
#10965 = CARTESIAN_POINT('Origin',(104.,25.5,25.5)) ;
#10966 = CARTESIAN_POINT('Origin',(120.,25.5,25.5)) ;
#10967 = CARTESIAN_POINT('',(120.,20.,25.5)) ;
#10968 = CARTESIAN_POINT('Origin',(120.,25.5,25.5)) ;
#10969 = CARTESIAN_POINT('Origin',(102.783257246469,25.5,25.5)) ;
#10970 = CARTESIAN_POINT('',(101.566514492938,25.5,25.5)) ;
#10971 = CARTESIAN_POINT('',(102.783257246469,23.475,25.5)) ;
#10972 = CARTESIAN_POINT('Origin',(0.25,25.5,25.5)) ;
#10973 = CARTESIAN_POINT('',(0.,25.5,30.05)) ;
#10974 = CARTESIAN_POINT('Origin',(0.,25.5,25.5)) ;
#10975 = CARTESIAN_POINT('',(0.5,25.5,29.55)) ;
#10976 = CARTESIAN_POINT('',(0.25,25.5,29.8)) ;
#10977 = CARTESIAN_POINT('Origin',(0.5,25.5,25.5)) ;
#10978 = CARTESIAN_POINT('Origin',(0.,25.5,25.5)) ;
#10979 = CARTESIAN_POINT('',(16.,25.5,29.55)) ;
#10980 = CARTESIAN_POINT('',(0.,25.5,29.55)) ;
#10981 = CARTESIAN_POINT('',(16.,21.45,25.5)) ;
#10982 = CARTESIAN_POINT('Origin',(16.,25.5,25.5)) ;
#10983 = CARTESIAN_POINT('Origin',(16.,25.5,25.5)) ;
#10984 = CARTESIAN_POINT('Origin',(0.,31.,25.5)) ;
#10985 = CARTESIAN_POINT('',(1.6306400674182E-15,20.,25.5)) ;
#10986 = CARTESIAN_POINT('Origin',(0.,25.5,25.5)) ;
#10987 = CARTESIAN_POINT('Origin',(16.,25.5,25.5)) ;
#10988 = CARTESIAN_POINT('',(18.4334855070616,25.5,25.5)) ;
#10989 = CARTESIAN_POINT('',(16.,21.45,25.5)) ;
#10990 = CARTESIAN_POINT('Origin',(118.,19.5,25.5)) ;
#10991 = CARTESIAN_POINT('',(118.,20.5,28.8166247903554)) ;
#10992 = CARTESIAN_POINT('',(118.,19.5,25.5)) ;
#10993 = CARTESIAN_POINT('Origin',(118.,25.5,25.5)) ;
#10994 = CARTESIAN_POINT('',(118.,20.5,22.1833752096446)) ;
#10995 = CARTESIAN_POINT('',(118.,20.5,32.5)) ;
#10996 = CARTESIAN_POINT('Origin',(118.,25.5,25.5)) ;
#10997 = CARTESIAN_POINT('Origin',(106.,20.5,18.5)) ;
#10998 = CARTESIAN_POINT('',(106.,20.5,28.8166247903554)) ;
#10999 = CARTESIAN_POINT('',(105.75,20.5,28.8166247903554)) ;
#11000 = CARTESIAN_POINT('',(106.,20.5,22.1833752096446)) ;
#11001 = CARTESIAN_POINT('',(106.,20.5,32.5)) ;
#11002 = CARTESIAN_POINT('',(105.75,20.5,22.1833752096446)) ;
#11003 = CARTESIAN_POINT('Origin',(106.,19.5,25.5)) ;
#11004 = CARTESIAN_POINT('',(106.,19.5,25.5)) ;
#11005 = CARTESIAN_POINT('Origin',(106.,25.5,25.5)) ;
#11006 = CARTESIAN_POINT('Origin',(106.,25.5,25.5)) ;
#11007 = CARTESIAN_POINT('Origin',(106.,31.5,25.5)) ;
#11008 = CARTESIAN_POINT('',(106.,30.5,28.8166247903554)) ;
#11009 = CARTESIAN_POINT('',(106.,30.5,22.1833752096446)) ;
#11010 = CARTESIAN_POINT('Origin',(106.,25.5,25.5)) ;
#11011 = CARTESIAN_POINT('',(106.,30.5,32.5)) ;
#11012 = CARTESIAN_POINT('Origin',(106.,30.5,32.5)) ;
#11013 = CARTESIAN_POINT('',(118.,30.5,28.8166247903554)) ;
#11014 = CARTESIAN_POINT('',(105.75,30.5,28.8166247903554)) ;
#11015 = CARTESIAN_POINT('',(118.,30.5,22.1833752096446)) ;
#11016 = CARTESIAN_POINT('',(118.,30.5,32.5)) ;
#11017 = CARTESIAN_POINT('',(105.75,30.5,22.1833752096446)) ;
#11018 = CARTESIAN_POINT('Origin',(118.,31.5,25.5)) ;
#11019 = CARTESIAN_POINT('Origin',(118.,25.5,25.5)) ;
#11020 = CARTESIAN_POINT('Origin',(12.,19.8431457505076,19.8431457505076)) ;
#11021 = CARTESIAN_POINT('',(92.,21.2911524926819,19.0520854022295)) ;
#11022 = CARTESIAN_POINT('',(91.7,21.1239700652888,18.802958712199)) ;
#11023 = CARTESIAN_POINT('Ctrl Pts',(92.,21.2911524926819,19.0520854022295)) ;
#11024 = CARTESIAN_POINT('Ctrl Pts',(91.9567026846615,21.2703306474521,19.0139717837895)) ;
#11025 = CARTESIAN_POINT('Ctrl Pts',(91.9139415332125,21.2483235990085,18.9772740185191)) ;
#11026 = CARTESIAN_POINT('Ctrl Pts',(91.8156742489856,21.1946634967733,18.8949511627776)) ;
#11027 = CARTESIAN_POINT('Ctrl Pts',(91.7581599879312,21.1608316055721,18.8483478156355)) ;
#11028 = CARTESIAN_POINT('Ctrl Pts',(91.7,21.1239700652888,18.802958712199)) ;
#11029 = CARTESIAN_POINT('',(92.,19.0520854022295,21.2911524926819)) ;
#11030 = CARTESIAN_POINT('Origin',(92.,19.8431457505076,19.8431457505076)) ;
#11031 = CARTESIAN_POINT('',(91.7,18.802958712199,21.1239700652888)) ;
#11032 = CARTESIAN_POINT('Ctrl Pts',(91.7,18.802958712199,21.1239700652888)) ;
#11033 = CARTESIAN_POINT('Ctrl Pts',(91.7581599873228,18.8483478151607,21.1608316051865)) ;
#11034 = CARTESIAN_POINT('Ctrl Pts',(91.8156742480668,18.8949511620079,21.1946634962716)) ;
#11035 = CARTESIAN_POINT('Ctrl Pts',(91.872005365357,18.9421422335728,21.2254238203876)) ;
#11036 = CARTESIAN_POINT('Ctrl Pts',(91.9139415332125,18.9772740185191,21.2483235990085)) ;
#11037 = CARTESIAN_POINT('Ctrl Pts',(91.9567026846615,19.0139717837895,21.2703306474521)) ;
#11038 = CARTESIAN_POINT('Ctrl Pts',(92.,19.0520854022295,21.2911524926819)) ;
#11039 = CARTESIAN_POINT('',(12.3,18.802958712199,21.1239700652888)) ;
#11040 = CARTESIAN_POINT('',(12.,18.802958712199,21.1239700652888)) ;
#11041 = CARTESIAN_POINT('',(12.,19.0520854022295,21.2911524926819)) ;
#11042 = CARTESIAN_POINT('Ctrl Pts',(12.,19.0520854022295,21.2911524926819)) ;
#11043 = CARTESIAN_POINT('Ctrl Pts',(12.0432973155239,19.0139717836263,21.2703306473629)) ;
#11044 = CARTESIAN_POINT('Ctrl Pts',(12.0860584670469,18.9772740183018,21.2483235988669)) ;
#11045 = CARTESIAN_POINT('Ctrl Pts',(12.127994634643,18.9421422335728,21.2254238203876)) ;
#11046 = CARTESIAN_POINT('Ctrl Pts',(12.1843257510144,18.8949511627776,21.1946634967733)) ;
#11047 = CARTESIAN_POINT('Ctrl Pts',(12.2418400120688,18.8483478156355,21.1608316055721)) ;
#11048 = CARTESIAN_POINT('Ctrl Pts',(12.3,18.802958712199,21.1239700652888)) ;
#11049 = CARTESIAN_POINT('',(12.,21.2911524926819,19.0520854022295)) ;
#11050 = CARTESIAN_POINT('Origin',(12.,19.8431457505076,19.8431457505076)) ;
#11051 = CARTESIAN_POINT('',(12.3,21.1239700652888,18.802958712199)) ;
#11052 = CARTESIAN_POINT('Ctrl Pts',(12.3,21.1239700652888,18.802958712199)) ;
#11053 = CARTESIAN_POINT('Ctrl Pts',(12.2418400120688,21.1608316055721,18.8483478156355)) ;
#11054 = CARTESIAN_POINT('Ctrl Pts',(12.1843257510144,21.1946634967733,18.8949511627776)) ;
#11055 = CARTESIAN_POINT('Ctrl Pts',(12.0860584667875,21.2483235990085,18.9772740185191)) ;
#11056 = CARTESIAN_POINT('Ctrl Pts',(12.0432973153384,21.2703306474521,19.0139717837895)) ;
#11057 = CARTESIAN_POINT('Ctrl Pts',(12.,21.2911524926819,19.0520854022295)) ;
#11058 = CARTESIAN_POINT('',(12.,21.1239700652888,18.802958712199)) ;
#11059 = CARTESIAN_POINT('Origin',(12.,31.1568542494924,19.8431457505076)) ;
#11060 = CARTESIAN_POINT('',(92.,31.9479145977705,21.2911524926819)) ;
#11061 = CARTESIAN_POINT('',(91.7,32.197041287801,21.1239700652888)) ;
#11062 = CARTESIAN_POINT('Ctrl Pts',(92.,31.9479145977705,21.2911524926819)) ;
#11063 = CARTESIAN_POINT('Ctrl Pts',(91.9567026846615,31.9860282162105,21.2703306474521)) ;
#11064 = CARTESIAN_POINT('Ctrl Pts',(91.9139415332125,32.0227259814809,21.2483235990085)) ;
#11065 = CARTESIAN_POINT('Ctrl Pts',(91.8156742489856,32.1050488372224,21.1946634967733)) ;
#11066 = CARTESIAN_POINT('Ctrl Pts',(91.7581599879312,32.1516521843645,21.1608316055721)) ;
#11067 = CARTESIAN_POINT('Ctrl Pts',(91.7,32.197041287801,21.1239700652888)) ;
#11068 = CARTESIAN_POINT('',(92.,29.7088475073181,19.0520854022295)) ;
#11069 = CARTESIAN_POINT('Origin',(92.,31.1568542494924,19.8431457505076)) ;
#11070 = CARTESIAN_POINT('',(91.7,29.8760299347112,18.802958712199)) ;
#11071 = CARTESIAN_POINT('Ctrl Pts',(91.7,29.8760299347112,18.802958712199)) ;
#11072 = CARTESIAN_POINT('Ctrl Pts',(91.7581599873228,29.8391683948135,18.8483478151607)) ;
#11073 = CARTESIAN_POINT('Ctrl Pts',(91.8156742480668,29.8053365037284,18.8949511620079)) ;
#11074 = CARTESIAN_POINT('Ctrl Pts',(91.872005365357,29.7745761796124,18.9421422335728)) ;
#11075 = CARTESIAN_POINT('Ctrl Pts',(91.9139415332125,29.7516764009915,18.9772740185191)) ;
#11076 = CARTESIAN_POINT('Ctrl Pts',(91.9567026846615,29.7296693525479,19.0139717837895)) ;
#11077 = CARTESIAN_POINT('Ctrl Pts',(92.,29.7088475073181,19.0520854022295)) ;
#11078 = CARTESIAN_POINT('',(12.3,29.8760299347112,18.802958712199)) ;
#11079 = CARTESIAN_POINT('',(12.,29.8760299347112,18.802958712199)) ;
#11080 = CARTESIAN_POINT('',(12.,29.7088475073181,19.0520854022295)) ;
#11081 = CARTESIAN_POINT('Ctrl Pts',(12.,29.7088475073181,19.0520854022295)) ;
#11082 = CARTESIAN_POINT('Ctrl Pts',(12.0432973155239,29.7296693526371,19.0139717836263)) ;
#11083 = CARTESIAN_POINT('Ctrl Pts',(12.0860584670469,29.7516764011331,18.9772740183018)) ;
#11084 = CARTESIAN_POINT('Ctrl Pts',(12.127994634643,29.7745761796124,18.9421422335728)) ;
#11085 = CARTESIAN_POINT('Ctrl Pts',(12.1843257510144,29.8053365032267,18.8949511627776)) ;
#11086 = CARTESIAN_POINT('Ctrl Pts',(12.2418400120688,29.8391683944279,18.8483478156355)) ;
#11087 = CARTESIAN_POINT('Ctrl Pts',(12.3,29.8760299347112,18.802958712199)) ;
#11088 = CARTESIAN_POINT('',(12.,31.9479145977705,21.2911524926819)) ;
#11089 = CARTESIAN_POINT('Origin',(12.,31.1568542494924,19.8431457505076)) ;
#11090 = CARTESIAN_POINT('',(12.3,32.197041287801,21.1239700652888)) ;
#11091 = CARTESIAN_POINT('Ctrl Pts',(12.3,32.197041287801,21.1239700652888)) ;
#11092 = CARTESIAN_POINT('Ctrl Pts',(12.2418400120688,32.1516521843645,21.1608316055721)) ;
#11093 = CARTESIAN_POINT('Ctrl Pts',(12.1843257510144,32.1050488372224,21.1946634967733)) ;
#11094 = CARTESIAN_POINT('Ctrl Pts',(12.0860584667875,32.0227259814809,21.2483235990085)) ;
#11095 = CARTESIAN_POINT('Ctrl Pts',(12.0432973153384,31.9860282162105,21.2703306474521)) ;
#11096 = CARTESIAN_POINT('Ctrl Pts',(12.,31.9479145977705,21.2911524926819)) ;
#11097 = CARTESIAN_POINT('',(12.,32.197041287801,21.1239700652888)) ;
#11098 = CARTESIAN_POINT('Origin',(12.,31.1568542494924,31.1568542494924)) ;
#11099 = CARTESIAN_POINT('',(91.7,32.197041287801,29.8760299347112)) ;
#11100 = CARTESIAN_POINT('',(92.,31.9479145977705,29.7088475073181)) ;
#11101 = CARTESIAN_POINT('Ctrl Pts',(91.7,32.197041287801,29.8760299347112)) ;
#11102 = CARTESIAN_POINT('Ctrl Pts',(91.7581599873228,32.1516521848393,29.8391683948135)) ;
#11103 = CARTESIAN_POINT('Ctrl Pts',(91.8156742480668,32.1050488379921,29.8053365037284)) ;
#11104 = CARTESIAN_POINT('Ctrl Pts',(91.872005365357,32.0578577664272,29.7745761796124)) ;
#11105 = CARTESIAN_POINT('Ctrl Pts',(91.9139415332125,32.0227259814809,29.7516764009914)) ;
#11106 = CARTESIAN_POINT('Ctrl Pts',(91.9567026846615,31.9860282162105,29.7296693525479)) ;
#11107 = CARTESIAN_POINT('Ctrl Pts',(92.,31.9479145977705,29.7088475073181)) ;
#11108 = CARTESIAN_POINT('',(12.3,32.197041287801,29.8760299347112)) ;
#11109 = CARTESIAN_POINT('',(12.,32.197041287801,29.8760299347112)) ;
#11110 = CARTESIAN_POINT('',(12.,31.9479145977705,29.7088475073181)) ;
#11111 = CARTESIAN_POINT('Ctrl Pts',(12.,31.9479145977705,29.7088475073181)) ;
#11112 = CARTESIAN_POINT('Ctrl Pts',(12.0432973155239,31.9860282163737,29.7296693526371)) ;
#11113 = CARTESIAN_POINT('Ctrl Pts',(12.0860584670469,32.0227259816982,29.7516764011331)) ;
#11114 = CARTESIAN_POINT('Ctrl Pts',(12.127994634643,32.0578577664272,29.7745761796124)) ;
#11115 = CARTESIAN_POINT('Ctrl Pts',(12.1843257510144,32.1050488372224,29.8053365032267)) ;
#11116 = CARTESIAN_POINT('Ctrl Pts',(12.2418400120688,32.1516521843645,29.8391683944279)) ;
#11117 = CARTESIAN_POINT('Ctrl Pts',(12.3,32.197041287801,29.8760299347112)) ;
#11118 = CARTESIAN_POINT('',(12.,29.7088475073181,31.9479145977705)) ;
#11119 = CARTESIAN_POINT('Origin',(12.,31.1568542494924,31.1568542494924)) ;
#11120 = CARTESIAN_POINT('',(12.3,29.8760299347112,32.197041287801)) ;
#11121 = CARTESIAN_POINT('Ctrl Pts',(12.3,29.8760299347112,32.197041287801)) ;
#11122 = CARTESIAN_POINT('Ctrl Pts',(12.2418400120688,29.8391683944279,32.1516521843645)) ;
#11123 = CARTESIAN_POINT('Ctrl Pts',(12.1843257510144,29.8053365032267,32.1050488372224)) ;
#11124 = CARTESIAN_POINT('Ctrl Pts',(12.0860584667875,29.7516764009915,32.0227259814809)) ;
#11125 = CARTESIAN_POINT('Ctrl Pts',(12.0432973153384,29.7296693525479,31.9860282162105)) ;
#11126 = CARTESIAN_POINT('Ctrl Pts',(12.,29.7088475073181,31.9479145977705)) ;
#11127 = CARTESIAN_POINT('',(91.7,29.8760299347112,32.197041287801)) ;
#11128 = CARTESIAN_POINT('',(12.,29.8760299347112,32.197041287801)) ;
#11129 = CARTESIAN_POINT('',(92.,29.7088475073181,31.9479145977705)) ;
#11130 = CARTESIAN_POINT('Ctrl Pts',(92.,29.7088475073181,31.9479145977705)) ;
#11131 = CARTESIAN_POINT('Ctrl Pts',(91.9567026846615,29.7296693525479,31.9860282162105)) ;
#11132 = CARTESIAN_POINT('Ctrl Pts',(91.9139415332125,29.7516764009915,32.0227259814809)) ;
#11133 = CARTESIAN_POINT('Ctrl Pts',(91.8156742489856,29.8053365032267,32.1050488372224)) ;
#11134 = CARTESIAN_POINT('Ctrl Pts',(91.7581599879312,29.8391683944279,32.1516521843645)) ;
#11135 = CARTESIAN_POINT('Ctrl Pts',(91.7,29.8760299347112,32.197041287801)) ;
#11136 = CARTESIAN_POINT('Origin',(92.,31.1568542494924,31.1568542494924)) ;
#11137 = CARTESIAN_POINT('Origin',(12.,19.8431457505076,31.1568542494924)) ;
#11138 = CARTESIAN_POINT('',(91.7,21.1239700652888,32.197041287801)) ;
#11139 = CARTESIAN_POINT('',(92.,21.2911524926819,31.9479145977705)) ;
#11140 = CARTESIAN_POINT('Ctrl Pts',(91.7,21.1239700652888,32.197041287801)) ;
#11141 = CARTESIAN_POINT('Ctrl Pts',(91.7581599873228,21.1608316051865,32.1516521848393)) ;
#11142 = CARTESIAN_POINT('Ctrl Pts',(91.8156742480668,21.1946634962716,32.1050488379921)) ;
#11143 = CARTESIAN_POINT('Ctrl Pts',(91.872005365357,21.2254238203876,32.0578577664272)) ;
#11144 = CARTESIAN_POINT('Ctrl Pts',(91.9139415332125,21.2483235990085,32.0227259814809)) ;
#11145 = CARTESIAN_POINT('Ctrl Pts',(91.9567026846616,21.2703306474521,31.9860282162104)) ;
#11146 = CARTESIAN_POINT('Ctrl Pts',(92.,21.2911524926819,31.9479145977705)) ;
#11147 = CARTESIAN_POINT('',(12.3,21.1239700652888,32.197041287801)) ;
#11148 = CARTESIAN_POINT('',(12.,21.1239700652888,32.197041287801)) ;
#11149 = CARTESIAN_POINT('',(12.,21.2911524926819,31.9479145977705)) ;
#11150 = CARTESIAN_POINT('Ctrl Pts',(12.,21.2911524926819,31.9479145977705)) ;
#11151 = CARTESIAN_POINT('Ctrl Pts',(12.0432973155239,21.2703306473629,31.9860282163737)) ;
#11152 = CARTESIAN_POINT('Ctrl Pts',(12.0860584670469,21.2483235988669,32.0227259816982)) ;
#11153 = CARTESIAN_POINT('Ctrl Pts',(12.127994634643,21.2254238203876,32.0578577664272)) ;
#11154 = CARTESIAN_POINT('Ctrl Pts',(12.1843257510144,21.1946634967733,32.1050488372224)) ;
#11155 = CARTESIAN_POINT('Ctrl Pts',(12.2418400120688,21.1608316055721,32.1516521843645)) ;
#11156 = CARTESIAN_POINT('Ctrl Pts',(12.3,21.1239700652888,32.197041287801)) ;
#11157 = CARTESIAN_POINT('',(12.,19.0520854022295,29.7088475073181)) ;
#11158 = CARTESIAN_POINT('Origin',(12.,19.8431457505076,31.1568542494924)) ;
#11159 = CARTESIAN_POINT('',(12.3,18.802958712199,29.8760299347112)) ;
#11160 = CARTESIAN_POINT('Ctrl Pts',(12.3,18.802958712199,29.8760299347112)) ;
#11161 = CARTESIAN_POINT('Ctrl Pts',(12.2418400120688,18.8483478156355,29.8391683944279)) ;
#11162 = CARTESIAN_POINT('Ctrl Pts',(12.1843257510144,18.8949511627776,29.8053365032267)) ;
#11163 = CARTESIAN_POINT('Ctrl Pts',(12.0860584667875,18.9772740185191,29.7516764009915)) ;
#11164 = CARTESIAN_POINT('Ctrl Pts',(12.0432973153384,19.0139717837895,29.7296693525479)) ;
#11165 = CARTESIAN_POINT('Ctrl Pts',(12.,19.0520854022295,29.7088475073181)) ;
#11166 = CARTESIAN_POINT('',(91.7,18.802958712199,29.8760299347112)) ;
#11167 = CARTESIAN_POINT('',(12.,18.802958712199,29.8760299347112)) ;
#11168 = CARTESIAN_POINT('',(92.,19.0520854022295,29.7088475073181)) ;
#11169 = CARTESIAN_POINT('Ctrl Pts',(92.,19.0520854022295,29.7088475073181)) ;
#11170 = CARTESIAN_POINT('Ctrl Pts',(91.9567026846615,19.0139717837895,29.7296693525479)) ;
#11171 = CARTESIAN_POINT('Ctrl Pts',(91.9139415332125,18.9772740185191,29.7516764009915)) ;
#11172 = CARTESIAN_POINT('Ctrl Pts',(91.8156742489856,18.8949511627776,29.8053365032267)) ;
#11173 = CARTESIAN_POINT('Ctrl Pts',(91.7581599879312,18.8483478156355,29.8391683944279)) ;
#11174 = CARTESIAN_POINT('Ctrl Pts',(91.7,18.802958712199,29.8760299347112)) ;
#11175 = CARTESIAN_POINT('Origin',(92.,19.8431457505076,31.1568542494924)) ;
#11176 = CARTESIAN_POINT('Origin',(91.85,25.5,25.5)) ;
#11177 = CARTESIAN_POINT('Origin',(91.7,25.5,25.5)) ;
#11178 = CARTESIAN_POINT('Origin',(92.,25.5,25.5)) ;
#11179 = CARTESIAN_POINT('Origin',(91.85,25.5,25.5)) ;
#11180 = CARTESIAN_POINT('Origin',(91.7,25.5,25.5)) ;
#11181 = CARTESIAN_POINT('Origin',(92.,25.5,25.5)) ;
#11182 = CARTESIAN_POINT('Origin',(91.85,25.5,25.5)) ;
#11183 = CARTESIAN_POINT('Origin',(92.,25.5,25.5)) ;
#11184 = CARTESIAN_POINT('Origin',(91.7,25.5,25.5)) ;
#11185 = CARTESIAN_POINT('Origin',(91.85,25.5,25.5)) ;
#11186 = CARTESIAN_POINT('Origin',(91.7,25.5,25.5)) ;
#11187 = CARTESIAN_POINT('Origin',(92.,25.5,25.5)) ;
#11188 = CARTESIAN_POINT('Origin',(52.,25.5,25.5)) ;
#11189 = CARTESIAN_POINT('Origin',(12.3,25.5,25.5)) ;
#11190 = CARTESIAN_POINT('Origin',(52.,25.5,25.5)) ;
#11191 = CARTESIAN_POINT('Origin',(12.3,25.5,25.5)) ;
#11192 = CARTESIAN_POINT('Origin',(52.,25.5,25.5)) ;
#11193 = CARTESIAN_POINT('Origin',(12.3,25.5,25.5)) ;
#11194 = CARTESIAN_POINT('Origin',(52.,25.5,25.5)) ;
#11195 = CARTESIAN_POINT('Origin',(12.3,25.5,25.5)) ;
#11196 = CARTESIAN_POINT('Origin',(12.15,25.5,25.5)) ;
#11197 = CARTESIAN_POINT('Origin',(12.,25.5,25.5)) ;
#11198 = CARTESIAN_POINT('Origin',(12.15,25.5,25.5)) ;
#11199 = CARTESIAN_POINT('Origin',(12.,25.5,25.5)) ;
#11200 = CARTESIAN_POINT('Origin',(12.15,25.5,25.5)) ;
#11201 = CARTESIAN_POINT('Origin',(12.,25.5,25.5)) ;
#11202 = CARTESIAN_POINT('Origin',(12.15,25.5,25.5)) ;
#11203 = CARTESIAN_POINT('Origin',(12.,25.5,25.5)) ;
#11204 = CARTESIAN_POINT('Origin',(12.,33.2,25.5)) ;
#11205 = CARTESIAN_POINT('',(12.,19.5,25.5)) ;
#11206 = CARTESIAN_POINT('Origin',(12.,25.5,25.5)) ;
#11207 = CARTESIAN_POINT('Origin',(0.250000000000004,25.5,25.5)) ;
#11208 = CARTESIAN_POINT('',(0.500000000000006,19.5,25.5)) ;
#11209 = CARTESIAN_POINT('Origin',(0.500000000000007,25.5,25.5)) ;
#11210 = CARTESIAN_POINT('',(0.250000000000004,19.75,25.5)) ;
#11211 = CARTESIAN_POINT('Origin',(6.25,25.5,25.5)) ;
#11212 = CARTESIAN_POINT('',(6.25,19.5,25.5)) ;
#11213 = CARTESIAN_POINT('Origin',(92.,31.5,25.5)) ;
#11214 = CARTESIAN_POINT('',(92.,19.5,25.5)) ;
#11215 = CARTESIAN_POINT('Origin',(92.,25.5,25.5)) ;
#11216 = CARTESIAN_POINT('Origin',(105.75,25.5,25.5)) ;
#11217 = CARTESIAN_POINT('',(119.5,19.5,25.5)) ;
#11218 = CARTESIAN_POINT('Origin',(119.5,25.5,25.5)) ;
#11219 = CARTESIAN_POINT('',(105.75,19.5,25.5)) ;
#11220 = CARTESIAN_POINT('',(105.75,19.5,25.5)) ;
#11221 = CARTESIAN_POINT('Origin',(119.75,25.5,25.5)) ;
#11222 = CARTESIAN_POINT('',(119.75,19.75,25.5)) ;
#11223 = CARTESIAN_POINT('',(0.,0.,0.)) ;
#11224 = CARTESIAN_POINT('Ctrl Pts',(66.2495224699378,41.5,26.4154158473015)) ;
#11225 = CARTESIAN_POINT('Ctrl Pts',(66.2495224699378,40.85,26.4154158473015)) ;
#11226 = CARTESIAN_POINT('Ctrl Pts',(66.4206003174186,41.5,26.4154158473015)) ;
#11227 = CARTESIAN_POINT('Ctrl Pts',(66.4206003174186,40.85,26.4154158473015)) ;
#11228 = CARTESIAN_POINT('Ctrl Pts',(66.5436561927199,41.5,26.277353310585)) ;
#11229 = CARTESIAN_POINT('Ctrl Pts',(66.5436561927199,40.85,26.277353310585)) ;
#11230 = CARTESIAN_POINT('',(66.2495224699378,40.9729445751773,26.4154158473015)) ;
#11231 = CARTESIAN_POINT('',(66.5436561927199,40.9804948832562,26.277353310585)) ;
#11232 = CARTESIAN_POINT('Ctrl Pts',(66.2495224699378,40.9729445751773,26.4154158473015)) ;
#11233 = CARTESIAN_POINT('Ctrl Pts',(66.2995225246323,40.9729445751773,26.4154158473015)) ;
#11234 = CARTESIAN_POINT('Ctrl Pts',(66.3478889016248,40.9734772686179,26.4065715531905)) ;
#11235 = CARTESIAN_POINT('Ctrl Pts',(66.3940330750068,40.9745795963019,26.3873479124433)) ;
#11236 = CARTESIAN_POINT('Ctrl Pts',(66.4219819653177,40.9752472609986,26.3757044179944)) ;
#11237 = CARTESIAN_POINT('Ctrl Pts',(66.4480801252716,40.9760959140079,26.3606844081376)) ;
#11238 = CARTESIAN_POINT('Ctrl Pts',(66.4724676043192,40.9770721634385,26.3427557461786)) ;
#11239 = CARTESIAN_POINT('Ctrl Pts',(66.4985095759234,40.978114643471,26.3236107699913)) ;
#11240 = CARTESIAN_POINT('Ctrl Pts',(66.5221553224869,40.979283551382,26.3014762114925)) ;
#11241 = CARTESIAN_POINT('Ctrl Pts',(66.5436561927199,40.9804948832562,26.277353310585)) ;
#11242 = CARTESIAN_POINT('',(66.2495224699378,40.85,26.4154158473015)) ;
#11243 = CARTESIAN_POINT('',(66.2495224699378,41.5,26.4154158473015)) ;
#11244 = CARTESIAN_POINT('',(66.5436561927199,40.85,26.277353310585)) ;
#11245 = CARTESIAN_POINT('Ctrl Pts',(66.2495224699378,40.85,26.4154158473015)) ;
#11246 = CARTESIAN_POINT('Ctrl Pts',(66.4206003174186,40.85,26.4154158473015)) ;
#11247 = CARTESIAN_POINT('Ctrl Pts',(66.5436561927199,40.85,26.277353310585)) ;
#11248 = CARTESIAN_POINT('',(66.5436561927199,41.5,26.277353310585)) ;
#11249 = CARTESIAN_POINT('Ctrl Pts',(66.5436561927199,41.5,26.277353310585)) ;
#11250 = CARTESIAN_POINT('Ctrl Pts',(66.5436561927199,40.85,26.277353310585)) ;
#11251 = CARTESIAN_POINT('Ctrl Pts',(66.6667120680213,41.5,26.1392904758453)) ;
#11252 = CARTESIAN_POINT('Ctrl Pts',(66.6667120680213,40.85,26.1392904758453)) ;
#11253 = CARTESIAN_POINT('Ctrl Pts',(66.6667120680213,41.5,25.9021826028824)) ;
#11254 = CARTESIAN_POINT('Ctrl Pts',(66.6667120680213,40.85,25.9021826028824)) ;
#11255 = CARTESIAN_POINT('',(66.6667120680213,40.9947813522469,25.9021826028824)) ;
#11256 = CARTESIAN_POINT('Ctrl Pts',(66.5436561927199,40.9804948832562,26.277353310585)) ;
#11257 = CARTESIAN_POINT('Ctrl Pts',(66.5821223532304,40.9826620228363,26.2341961094468)) ;
#11258 = CARTESIAN_POINT('Ctrl Pts',(66.6105875841343,40.9849568963094,26.1848827603603)) ;
#11259 = CARTESIAN_POINT('Ctrl Pts',(66.6303948051965,40.9871681759971,26.1305726670125)) ;
#11260 = CARTESIAN_POINT('Ctrl Pts',(66.6499886361015,40.9893556327912,26.076847675397)) ;
#11261 = CARTESIAN_POINT('Ctrl Pts',(66.6604621061239,40.9913728985934,26.0199931986045)) ;
#11262 = CARTESIAN_POINT('Ctrl Pts',(66.6645899528845,40.9930871506489,25.9627489167057)) ;
#11263 = CARTESIAN_POINT('Ctrl Pts',(66.6660451595907,40.9936914829393,25.9425683558126)) ;
#11264 = CARTESIAN_POINT('Ctrl Pts',(66.6667120680213,40.9942581565947,25.9223396215523)) ;
#11265 = CARTESIAN_POINT('Ctrl Pts',(66.6667120680213,40.9947813522469,25.9021826028824)) ;
#11266 = CARTESIAN_POINT('',(66.6667120680213,40.85,25.9021826028824)) ;
#11267 = CARTESIAN_POINT('Ctrl Pts',(66.5436561927199,40.85,26.277353310585)) ;
#11268 = CARTESIAN_POINT('Ctrl Pts',(66.6667120680213,40.85,26.1392904758453)) ;
#11269 = CARTESIAN_POINT('Ctrl Pts',(66.6667120680213,40.85,25.9021826028824)) ;
#11270 = CARTESIAN_POINT('',(66.6667120680213,41.5,25.9021826028824)) ;
#11271 = CARTESIAN_POINT('Ctrl Pts',(66.6667120680213,41.5,25.9021826028824)) ;
#11272 = CARTESIAN_POINT('Ctrl Pts',(66.6667120680213,40.85,25.9021826028824)) ;
#11273 = CARTESIAN_POINT('Ctrl Pts',(66.6667120680213,41.5,25.6740789055824)) ;
#11274 = CARTESIAN_POINT('Ctrl Pts',(66.6667120680213,40.85,25.6740789055824)) ;
#11275 = CARTESIAN_POINT('Ctrl Pts',(66.5451570376754,41.5,25.5427692770958)) ;
#11276 = CARTESIAN_POINT('Ctrl Pts',(66.5451570376754,40.85,25.5427692770958)) ;
#11277 = CARTESIAN_POINT('',(66.5451570376754,40.9999409930792,25.5427692770958)) ;
#11278 = CARTESIAN_POINT('Ctrl Pts',(66.6667120680213,40.9947813522469,25.9021826028824)) ;
#11279 = CARTESIAN_POINT('Ctrl Pts',(66.6667120680213,40.9965684739587,25.8333306436577)) ;
#11280 = CARTESIAN_POINT('Ctrl Pts',(66.6584071624267,40.997895970425,25.7635943278561)) ;
#11281 = CARTESIAN_POINT('Ctrl Pts',(66.6363375933712,40.9987312162041,25.6983196608033)) ;
#11282 = CARTESIAN_POINT('Ctrl Pts',(66.6264687443208,40.9991047130536,25.6691307883633)) ;
#11283 = CARTESIAN_POINT('Ctrl Pts',(66.613931069591,40.999380770686,25.6410760408134)) ;
#11284 = CARTESIAN_POINT('Ctrl Pts',(66.5983483633277,40.9995771384542,25.6144924849394)) ;
#11285 = CARTESIAN_POINT('Ctrl Pts',(66.5832078919034,40.9997679333349,25.5886633663468)) ;
#11286 = CARTESIAN_POINT('Ctrl Pts',(66.5654960787534,40.9998803674897,25.5647404939194)) ;
#11287 = CARTESIAN_POINT('Ctrl Pts',(66.5451570376754,40.9999409930792,25.5427692770958)) ;
#11288 = CARTESIAN_POINT('',(66.5451570376754,40.85,25.5427692770958)) ;
#11289 = CARTESIAN_POINT('Ctrl Pts',(66.6667120680213,40.85,25.9021826028824)) ;
#11290 = CARTESIAN_POINT('Ctrl Pts',(66.6667120680213,40.85,25.6740789055824)) ;
#11291 = CARTESIAN_POINT('Ctrl Pts',(66.5451570376754,40.85,25.5427692770958)) ;
#11292 = CARTESIAN_POINT('',(66.5451570376754,41.5,25.5427692770958)) ;
#11293 = CARTESIAN_POINT('Ctrl Pts',(66.5451570376754,41.5,25.5427692770958)) ;
#11294 = CARTESIAN_POINT('Ctrl Pts',(66.5451570376754,40.85,25.5427692770958)) ;
#11295 = CARTESIAN_POINT('Ctrl Pts',(66.4236017093062,41.5,25.4114596486092)) ;
#11296 = CARTESIAN_POINT('Ctrl Pts',(66.4236017093062,40.85,25.4114596486092)) ;
#11297 = CARTESIAN_POINT('Ctrl Pts',(66.2390177473426,41.5,25.4114596486092)) ;
#11298 = CARTESIAN_POINT('Ctrl Pts',(66.2390177473426,40.85,25.4114596486092)) ;
#11299 = CARTESIAN_POINT('',(66.2390177473426,40.9997471142653,25.4114596486092)) ;
#11300 = CARTESIAN_POINT('Ctrl Pts',(66.5451570376754,40.9999409930792,25.5427692770958)) ;
#11301 = CARTESIAN_POINT('Ctrl Pts',(66.5082425374556,41.000051025693,25.5028925446262)) ;
#11302 = CARTESIAN_POINT('Ctrl Pts',(66.4655429676267,40.9999885189357,25.4705584633671)) ;
#11303 = CARTESIAN_POINT('Ctrl Pts',(66.4161246072134,40.9999126252241,25.4479556879396)) ;
#11304 = CARTESIAN_POINT('Ctrl Pts',(66.389129448404,40.9998711677015,25.4356087483184)) ;
#11305 = CARTESIAN_POINT('Ctrl Pts',(66.3610245827433,40.9998272455883,25.4265748528042)) ;
#11306 = CARTESIAN_POINT('Ctrl Pts',(66.3319507146315,40.999796548506,25.4205836608745)) ;
#11307 = CARTESIAN_POINT('Ctrl Pts',(66.301358198468,40.9997642479885,25.4142795242786)) ;
#11308 = CARTESIAN_POINT('Ctrl Pts',(66.2702519538158,40.9997471142653,25.4114596486092)) ;
#11309 = CARTESIAN_POINT('Ctrl Pts',(66.2390177473426,40.9997471142653,25.4114596486092)) ;
#11310 = CARTESIAN_POINT('',(66.2390177473426,40.85,25.4114596486092)) ;
#11311 = CARTESIAN_POINT('Ctrl Pts',(66.5451570376754,40.85,25.5427692770958)) ;
#11312 = CARTESIAN_POINT('Ctrl Pts',(66.4236017093062,40.85,25.4114596486092)) ;
#11313 = CARTESIAN_POINT('Ctrl Pts',(66.2390177473426,40.85,25.4114596486092)) ;
#11314 = CARTESIAN_POINT('',(66.2390177473426,41.5,25.4114596486092)) ;
#11315 = CARTESIAN_POINT('Ctrl Pts',(66.2930422052741,41.5,25.172851228714)) ;
#11316 = CARTESIAN_POINT('Ctrl Pts',(66.2930422052741,40.85,25.172851228714)) ;
#11317 = CARTESIAN_POINT('Ctrl Pts',(66.5631650909781,41.5,25.172851228714)) ;
#11318 = CARTESIAN_POINT('Ctrl Pts',(66.5631650909781,40.85,25.172851228714)) ;
#11319 = CARTESIAN_POINT('Ctrl Pts',(66.7530014142394,41.5,25.371691429615)) ;
#11320 = CARTESIAN_POINT('Ctrl Pts',(66.7530014142394,40.85,25.371691429615)) ;
#11321 = CARTESIAN_POINT('',(66.2930422052741,40.9965471535257,25.172851228714)) ;
#11322 = CARTESIAN_POINT('',(66.7530014142394,40.9994689235072,25.371691429615)) ;
#11323 = CARTESIAN_POINT('Ctrl Pts',(66.2930422052741,40.9965471535257,25.172851228714)) ;
#11324 = CARTESIAN_POINT('Ctrl Pts',(66.3770902451354,40.9965471535257,25.172851228714)) ;
#11325 = CARTESIAN_POINT('Ctrl Pts',(66.4586948235472,40.9968790271012,25.1872883524376)) ;
#11326 = CARTESIAN_POINT('Ctrl Pts',(66.5362595609816,40.9974645836146,25.2196582806458)) ;
#11327 = CARTESIAN_POINT('Ctrl Pts',(66.5764466645678,40.9977679665827,25.2364294797887)) ;
#11328 = CARTESIAN_POINT('Ctrl Pts',(66.6143004551277,40.998122981106,25.2574932807612)) ;
#11329 = CARTESIAN_POINT('Ctrl Pts',(66.6499502310137,40.9984739132174,25.2824997440933)) ;
#11330 = CARTESIAN_POINT('Ctrl Pts',(66.6872709183778,40.9988412935807,25.3086782649088)) ;
#11331 = CARTESIAN_POINT('Ctrl Pts',(66.7215222344078,40.9991959709695,25.3387192020962)) ;
#11332 = CARTESIAN_POINT('Ctrl Pts',(66.7530014142394,40.9994689235072,25.371691429615)) ;
#11333 = CARTESIAN_POINT('',(66.2930422052741,40.85,25.172851228714)) ;
#11334 = CARTESIAN_POINT('',(66.2930422052741,41.5,25.172851228714)) ;
#11335 = CARTESIAN_POINT('',(66.7530014142394,40.85,25.371691429615)) ;
#11336 = CARTESIAN_POINT('Ctrl Pts',(66.2930422052741,40.85,25.172851228714)) ;
#11337 = CARTESIAN_POINT('Ctrl Pts',(66.5631650909781,40.85,25.172851228714)) ;
#11338 = CARTESIAN_POINT('Ctrl Pts',(66.7530014142394,40.85,25.371691429615)) ;
#11339 = CARTESIAN_POINT('',(66.7530014142394,41.5,25.371691429615)) ;
#11340 = CARTESIAN_POINT('Ctrl Pts',(66.7530014142394,41.5,25.371691429615)) ;
#11341 = CARTESIAN_POINT('Ctrl Pts',(66.7530014142394,40.85,25.371691429615)) ;
#11342 = CARTESIAN_POINT('Ctrl Pts',(66.9428374394774,41.5,25.5705319285393)) ;
#11343 = CARTESIAN_POINT('Ctrl Pts',(66.9428374394774,40.85,25.5705319285393)) ;
#11344 = CARTESIAN_POINT('Ctrl Pts',(66.9428374394774,41.5,25.8856750965118)) ;
#11345 = CARTESIAN_POINT('Ctrl Pts',(66.9428374394774,40.85,25.8856750965118)) ;
#11346 = CARTESIAN_POINT('',(66.9428374394774,40.9952010222498,25.8856750965118)) ;
#11347 = CARTESIAN_POINT('Ctrl Pts',(66.7530014142394,40.9994689235072,25.371691429615)) ;
#11348 = CARTESIAN_POINT('Ctrl Pts',(66.8141251609826,40.9999989224803,25.4357144530812)) ;
#11349 = CARTESIAN_POINT('Ctrl Pts',(66.8606682486204,41.0002177343997,25.5089691574663)) ;
#11350 = CARTESIAN_POINT('Ctrl Pts',(66.8923690068865,40.9997292569968,25.5916130983996)) ;
#11351 = CARTESIAN_POINT('Ctrl Pts',(66.9283689303448,40.9991745337007,25.6854649716862)) ;
#11352 = CARTESIAN_POINT('Ctrl Pts',(66.9428374394774,40.997701693568,25.7852060615196)) ;
#11353 = CARTESIAN_POINT('Ctrl Pts',(66.9428374394774,40.9952010222498,25.8856750965118)) ;
#11354 = CARTESIAN_POINT('',(66.9428374394774,40.85,25.8856750965118)) ;
#11355 = CARTESIAN_POINT('Ctrl Pts',(66.7530014142394,40.85,25.371691429615)) ;
#11356 = CARTESIAN_POINT('Ctrl Pts',(66.9428374394774,40.85,25.5705319285393)) ;
#11357 = CARTESIAN_POINT('Ctrl Pts',(66.9428374394774,40.85,25.8856750965118)) ;
#11358 = CARTESIAN_POINT('',(66.9428374394774,41.5,25.8856750965118)) ;
#11359 = CARTESIAN_POINT('Ctrl Pts',(66.9428374394774,41.5,25.8856750965118)) ;
#11360 = CARTESIAN_POINT('Ctrl Pts',(66.9428374394774,40.85,25.8856750965118)) ;
#11361 = CARTESIAN_POINT('Ctrl Pts',(66.9428374394774,41.5,26.0927693486214)) ;
#11362 = CARTESIAN_POINT('Ctrl Pts',(66.9428374394774,40.85,26.0927693486214)) ;
#11363 = CARTESIAN_POINT('Ctrl Pts',(66.8535469993949,41.5,26.270600104332)) ;
#11364 = CARTESIAN_POINT('Ctrl Pts',(66.8535469993949,40.85,26.270600104332)) ;
#11365 = CARTESIAN_POINT('',(66.8535469993949,40.9808325189314,26.270600104332)) ;
#11366 = CARTESIAN_POINT('Ctrl Pts',(66.9428374394774,40.9952010222498,25.8856750965118)) ;
#11367 = CARTESIAN_POINT('Ctrl Pts',(66.9428374394774,40.9935236896344,25.9530649961756)) ;
#11368 = CARTESIAN_POINT('Ctrl Pts',(66.9357463397121,40.9914218942895,26.0197695444074)) ;
#11369 = CARTESIAN_POINT('Ctrl Pts',(66.9205286843305,40.9889416737403,26.0853937371291)) ;
#11370 = CARTESIAN_POINT('Ctrl Pts',(66.9055916133819,40.9865071837101,26.1498079453662)) ;
#11371 = CARTESIAN_POINT('Ctrl Pts',(66.8832087746672,40.9837731043684,26.2115257408558)) ;
#11372 = CARTESIAN_POINT('Ctrl Pts',(66.8535469993949,40.9808325189314,26.270600104332)) ;
#11373 = CARTESIAN_POINT('',(66.8535469993949,40.85,26.270600104332)) ;
#11374 = CARTESIAN_POINT('Ctrl Pts',(66.9428374394774,40.85,25.8856750965118)) ;
#11375 = CARTESIAN_POINT('Ctrl Pts',(66.9428374394774,40.85,26.0927693486214)) ;
#11376 = CARTESIAN_POINT('Ctrl Pts',(66.8535469993949,40.85,26.270600104332)) ;
#11377 = CARTESIAN_POINT('',(66.8535469993949,41.5,26.270600104332)) ;
#11378 = CARTESIAN_POINT('Ctrl Pts',(66.8535469993949,41.5,26.270600104332)) ;
#11379 = CARTESIAN_POINT('Ctrl Pts',(66.8535469993949,40.85,26.270600104332)) ;
#11380 = CARTESIAN_POINT('Ctrl Pts',(66.7642565593123,41.5,26.4484308600426)) ;
#11381 = CARTESIAN_POINT('Ctrl Pts',(66.7642565593123,40.85,26.4484308600426)) ;
#11382 = CARTESIAN_POINT('Ctrl Pts',(66.6081853732467,41.5,26.542973959446)) ;
#11383 = CARTESIAN_POINT('Ctrl Pts',(66.6081853732467,40.85,26.542973959446)) ;
#11384 = CARTESIAN_POINT('',(66.6081853732467,40.9648700388952,26.542973959446)) ;
#11385 = CARTESIAN_POINT('Ctrl Pts',(66.8535469993949,40.9808325189314,26.270600104332)) ;
#11386 = CARTESIAN_POINT('Ctrl Pts',(66.8250381231084,40.9780062286752,26.3273783552825)) ;
#11387 = CARTESIAN_POINT('Ctrl Pts',(66.7901650255163,40.9750546868546,26.3802952508486)) ;
#11388 = CARTESIAN_POINT('Ctrl Pts',(66.747650047791,40.9722242840042,26.4275104880653)) ;
#11389 = CARTESIAN_POINT('Ctrl Pts',(66.7068356273123,40.9695070944809,26.4728371622837)) ;
#11390 = CARTESIAN_POINT('Ctrl Pts',(66.66037489326,40.9670021881262,26.5113591617192)) ;
#11391 = CARTESIAN_POINT('Ctrl Pts',(66.6081853732467,40.9648700388952,26.542973959446)) ;
#11392 = CARTESIAN_POINT('',(66.6081853732467,40.85,26.542973959446)) ;
#11393 = CARTESIAN_POINT('Ctrl Pts',(66.8535469993949,40.85,26.270600104332)) ;
#11394 = CARTESIAN_POINT('Ctrl Pts',(66.7642565593123,40.85,26.4484308600426)) ;
#11395 = CARTESIAN_POINT('Ctrl Pts',(66.6081853732467,40.85,26.542973959446)) ;
#11396 = CARTESIAN_POINT('',(66.6081853732467,41.5,26.542973959446)) ;
#11397 = CARTESIAN_POINT('Ctrl Pts',(66.6081853732467,41.5,26.542973959446)) ;
#11398 = CARTESIAN_POINT('Ctrl Pts',(66.6081853732467,40.85,26.542973959446)) ;
#11399 = CARTESIAN_POINT('Ctrl Pts',(66.4521144852042,41.5,26.6375167608261)) ;
#11400 = CARTESIAN_POINT('Ctrl Pts',(66.4521144852042,40.85,26.6375167608261)) ;
#11401 = CARTESIAN_POINT('Ctrl Pts',(66.2540247067809,41.5,26.6375167608261)) ;
#11402 = CARTESIAN_POINT('Ctrl Pts',(66.2540247067809,40.85,26.6375167608261)) ;
#11403 = CARTESIAN_POINT('',(66.2540247067809,40.9582035055449,26.6375167608261)) ;
#11404 = CARTESIAN_POINT('Ctrl Pts',(66.6081853732467,40.9648700388952,26.542973959446)) ;
#11405 = CARTESIAN_POINT('Ctrl Pts',(66.5560744050866,40.962741101465,26.5745411336594)) ;
#11406 = CARTESIAN_POINT('Ctrl Pts',(66.500554898558,40.9610587138301,26.5981402654571)) ;
#11407 = CARTESIAN_POINT('Ctrl Pts',(66.4416646695438,40.9599256674031,26.613866400593)) ;
#11408 = CARTESIAN_POINT('Ctrl Pts',(66.3803551756684,40.9587460743851,26.6302385798481)) ;
#11409 = CARTESIAN_POINT('Ctrl Pts',(66.3174911111484,40.9582035055449,26.6375167608261)) ;
#11410 = CARTESIAN_POINT('Ctrl Pts',(66.2540247067809,40.9582035055449,26.6375167608261)) ;
#11411 = CARTESIAN_POINT('',(66.2540247067809,40.85,26.6375167608261)) ;
#11412 = CARTESIAN_POINT('Ctrl Pts',(66.6081853732467,40.85,26.542973959446)) ;
#11413 = CARTESIAN_POINT('Ctrl Pts',(66.4521144852042,40.85,26.6375167608261)) ;
#11414 = CARTESIAN_POINT('Ctrl Pts',(66.2540247067809,40.85,26.6375167608261)) ;
#11415 = CARTESIAN_POINT('',(66.2540247067809,41.5,26.6375167608261)) ;
#11416 = CARTESIAN_POINT('Ctrl Pts',(66.2540247067809,41.5,26.6375167608261)) ;
#11417 = CARTESIAN_POINT('Ctrl Pts',(66.2540247067809,40.85,26.6375167608261)) ;
#11418 = CARTESIAN_POINT('Ctrl Pts',(65.9163710996509,41.5,26.6375167608261)) ;
#11419 = CARTESIAN_POINT('Ctrl Pts',(65.9163710996509,40.85,26.6375167608261)) ;
#11420 = CARTESIAN_POINT('Ctrl Pts',(65.7032742127776,41.5,26.3891540408134)) ;
#11421 = CARTESIAN_POINT('Ctrl Pts',(65.7032742127776,40.85,26.3891540408134)) ;
#11422 = CARTESIAN_POINT('',(65.7032742127776,40.9744759230064,26.3891540408134)) ;
#11423 = CARTESIAN_POINT('Ctrl Pts',(66.2540247067809,40.9582035055449,26.6375167608261)) ;
#11424 = CARTESIAN_POINT('Ctrl Pts',(66.1548439595539,40.9582035055449,26.6375167608261)) ;
#11425 = CARTESIAN_POINT('Ctrl Pts',(66.0577652439653,40.9594243783883,26.6214479538109)) ;
#11426 = CARTESIAN_POINT('Ctrl Pts',(65.9661626126997,40.9620840160781,26.5834933685731)) ;
#11427 = CARTESIAN_POINT('Ctrl Pts',(65.9161152714711,40.9635371162038,26.5627567799801)) ;
#11428 = CARTESIAN_POINT('Ctrl Pts',(65.8693746381324,40.9653603683843,26.5361801946976)) ;
#11429 = CARTESIAN_POINT('Ctrl Pts',(65.8258305111509,40.9674499706989,26.503987750885)) ;
#11430 = CARTESIAN_POINT('Ctrl Pts',(65.7805849393146,40.9696212222128,26.4705374183124)) ;
#11431 = CARTESIAN_POINT('Ctrl Pts',(65.7399057668323,40.9720227639775,26.4318478245509)) ;
#11432 = CARTESIAN_POINT('Ctrl Pts',(65.7032742127776,40.9744759230064,26.3891540408134)) ;
#11433 = CARTESIAN_POINT('',(65.7032742127776,40.85,26.3891540408134)) ;
#11434 = CARTESIAN_POINT('Ctrl Pts',(66.2540247067809,40.85,26.6375167608261)) ;
#11435 = CARTESIAN_POINT('Ctrl Pts',(65.9163710996509,40.85,26.6375167608261)) ;
#11436 = CARTESIAN_POINT('Ctrl Pts',(65.7032742127776,40.85,26.3891540408134)) ;
#11437 = CARTESIAN_POINT('',(65.7032742127776,41.5,26.3891540408134)) ;
#11438 = CARTESIAN_POINT('Ctrl Pts',(65.7032742127776,41.5,26.3891540408134)) ;
#11439 = CARTESIAN_POINT('Ctrl Pts',(65.7032742127776,40.85,26.3891540408134)) ;
#11440 = CARTESIAN_POINT('Ctrl Pts',(65.4901773259044,41.5,26.1407910227776)) ;
#11441 = CARTESIAN_POINT('Ctrl Pts',(65.4901773259044,40.85,26.1407910227776)) ;
#11442 = CARTESIAN_POINT('Ctrl Pts',(65.4901773259044,41.5,25.5705319285393)) ;
#11443 = CARTESIAN_POINT('Ctrl Pts',(65.4901773259044,40.85,25.5705319285393)) ;
#11444 = CARTESIAN_POINT('',(65.4901773259044,40.9998395232679,25.5705319285393)) ;
#11445 = CARTESIAN_POINT('Ctrl Pts',(65.7032742127776,40.9744759230064,26.3891540408134)) ;
#11446 = CARTESIAN_POINT('Ctrl Pts',(65.6506026346571,40.9780032620947,26.3277656634483)) ;
#11447 = CARTESIAN_POINT('Ctrl Pts',(65.6114170771088,40.9817382887103,26.2559550399376)) ;
#11448 = CARTESIAN_POINT('Ctrl Pts',(65.5095628589581,40.9932219304136,25.9946808285601)) ;
#11449 = CARTESIAN_POINT('Ctrl Pts',(65.4901773259044,40.9989319317972,25.7699809219056)) ;
#11450 = CARTESIAN_POINT('Ctrl Pts',(65.4901773259044,40.9998395232679,25.5705319285393)) ;
#11451 = CARTESIAN_POINT('',(65.4901773259044,40.85,25.5705319285393)) ;
#11452 = CARTESIAN_POINT('Ctrl Pts',(65.7032742127776,40.85,26.3891540408134)) ;
#11453 = CARTESIAN_POINT('Ctrl Pts',(65.4901773259044,40.85,26.1407910227776)) ;
#11454 = CARTESIAN_POINT('Ctrl Pts',(65.4901773259044,40.85,25.5705319285393)) ;
#11455 = CARTESIAN_POINT('',(65.4901773259044,41.5,25.5705319285393)) ;
#11456 = CARTESIAN_POINT('Ctrl Pts',(65.4901773259044,41.5,25.5705319285393)) ;
#11457 = CARTESIAN_POINT('Ctrl Pts',(65.4901773259044,40.85,25.5705319285393)) ;
#11458 = CARTESIAN_POINT('Ctrl Pts',(65.4901773259044,41.5,24.9327419638634)) ;
#11459 = CARTESIAN_POINT('Ctrl Pts',(65.4901773259044,40.85,24.9327419638634)) ;
#11460 = CARTESIAN_POINT('Ctrl Pts',(65.7257843539119,41.5,24.6431103289127)) ;
#11461 = CARTESIAN_POINT('Ctrl Pts',(65.7257843539119,40.85,24.6431103289127)) ;
#11462 = CARTESIAN_POINT('',(65.7257843539119,40.9762960714631,24.6431103289127)) ;
#11463 = CARTESIAN_POINT('Ctrl Pts',(65.4901773259044,40.9998395232679,25.5705319285393)) ;
#11464 = CARTESIAN_POINT('Ctrl Pts',(65.4901773259044,41.0006654854803,25.3890214834158)) ;
#11465 = CARTESIAN_POINT('Ctrl Pts',(65.5044117837423,40.9980094292655,25.1956347335121)) ;
#11466 = CARTESIAN_POINT('Ctrl Pts',(65.5673107019122,40.9903345932874,24.9480044597343)) ;
#11467 = CARTESIAN_POINT('Ctrl Pts',(65.5912320855921,40.9876113571461,24.8767797364898)) ;
#11468 = CARTESIAN_POINT('Ctrl Pts',(65.6505396584418,40.9819752858246,24.7503534890286)) ;
#11469 = CARTESIAN_POINT('Ctrl Pts',(65.6844211051244,40.9791114077331,24.6939581557985)) ;
#11470 = CARTESIAN_POINT('Ctrl Pts',(65.7257843539119,40.9762960714631,24.6431103289127)) ;
#11471 = CARTESIAN_POINT('',(65.7257843539119,40.85,24.6431103289127)) ;
#11472 = CARTESIAN_POINT('Ctrl Pts',(65.4901773259044,40.85,25.5705319285393)) ;
#11473 = CARTESIAN_POINT('Ctrl Pts',(65.4901773259044,40.85,24.9327419638634)) ;
#11474 = CARTESIAN_POINT('Ctrl Pts',(65.7257843539119,40.85,24.6431103289127)) ;
#11475 = CARTESIAN_POINT('',(65.7257843539119,41.5,24.6431103289127)) ;
#11476 = CARTESIAN_POINT('Ctrl Pts',(65.7257843539119,41.5,24.6431103289127)) ;
#11477 = CARTESIAN_POINT('Ctrl Pts',(65.7257843539119,40.85,24.6431103289127)) ;
#11478 = CARTESIAN_POINT('Ctrl Pts',(65.9313779100776,41.5,24.3909957945347)) ;
#11479 = CARTESIAN_POINT('Ctrl Pts',(65.9313779100776,40.85,24.3909957945347)) ;
#11480 = CARTESIAN_POINT('Ctrl Pts',(66.2795360907912,41.5,24.3909957945347)) ;
#11481 = CARTESIAN_POINT('Ctrl Pts',(66.2795360907912,40.85,24.3909957945347)) ;
#11482 = CARTESIAN_POINT('',(66.2795360907912,40.9602752133414,24.3909957945347)) ;
#11483 = CARTESIAN_POINT('Ctrl Pts',(65.7257843539119,40.9762960714631,24.6431103289127)) ;
#11484 = CARTESIAN_POINT('Ctrl Pts',(65.7828697153532,40.9724201852525,24.5731078950428)) ;
#11485 = CARTESIAN_POINT('Ctrl Pts',(65.8503581339868,40.9687321451926,24.5150347541818)) ;
#11486 = CARTESIAN_POINT('Ctrl Pts',(65.9300081545895,40.9658953545615,24.4723420404865)) ;
#11487 = CARTESIAN_POINT('Ctrl Pts',(65.9816166823416,40.9640572811135,24.4446796735105)) ;
#11488 = CARTESIAN_POINT('Ctrl Pts',(66.0361961405409,40.9626560029032,24.4246179460631)) ;
#11489 = CARTESIAN_POINT('Ctrl Pts',(66.0932472026151,40.9617209739421,24.4113381957841)) ;
#11490 = CARTESIAN_POINT('Ctrl Pts',(66.1543031375699,40.9607203077783,24.3971262330306)) ;
#11491 = CARTESIAN_POINT('Ctrl Pts',(66.216844930776,40.9602752133414,24.3909957945347)) ;
#11492 = CARTESIAN_POINT('Ctrl Pts',(66.2795360907912,40.9602752133414,24.3909957945347)) ;
#11493 = CARTESIAN_POINT('',(66.2795360907912,40.85,24.3909957945347)) ;
#11494 = CARTESIAN_POINT('Ctrl Pts',(65.7257843539119,40.85,24.6431103289127)) ;
#11495 = CARTESIAN_POINT('Ctrl Pts',(65.9313779100776,40.85,24.3909957945347)) ;
#11496 = CARTESIAN_POINT('Ctrl Pts',(66.2795360907912,40.85,24.3909957945347)) ;
#11497 = CARTESIAN_POINT('',(66.2795360907912,41.5,24.3909957945347)) ;
#11498 = CARTESIAN_POINT('Ctrl Pts',(66.2390177473426,41.5,25.4114596486092)) ;
#11499 = CARTESIAN_POINT('Ctrl Pts',(66.2390177473426,40.85,25.4114596486092)) ;
#11500 = CARTESIAN_POINT('Ctrl Pts',(66.0559344813228,41.5,25.4114596486092)) ;
#11501 = CARTESIAN_POINT('Ctrl Pts',(66.0559344813228,40.85,25.4114596486092)) ;
#11502 = CARTESIAN_POINT('Ctrl Pts',(65.9283765181899,41.5,25.5427692770958)) ;
#11503 = CARTESIAN_POINT('Ctrl Pts',(65.9283765181899,40.85,25.5427692770958)) ;
#11504 = CARTESIAN_POINT('',(65.9283765181899,40.9999409930792,25.5427692770958)) ;
#11505 = CARTESIAN_POINT('Ctrl Pts',(66.2390177473426,40.9997471142653,25.4114596486092)) ;
#11506 = CARTESIAN_POINT('Ctrl Pts',(66.1805248823561,40.9997471142653,25.4114596486092)) ;
#11507 = CARTESIAN_POINT('Ctrl Pts',(66.1236953715062,40.9998180096227,25.4215118920112)) ;
#11508 = CARTESIAN_POINT('Ctrl Pts',(66.0698158208354,40.9998998728118,25.4442870499013)) ;
#11509 = CARTESIAN_POINT('Ctrl Pts',(66.0159384991141,40.9999817326143,25.4670612656033)) ;
#11510 = CARTESIAN_POINT('Ctrl Pts',(65.9691314140412,41.0000567563128,25.5008157204395)) ;
#11511 = CARTESIAN_POINT('Ctrl Pts',(65.9283765181899,40.9999409930792,25.5427692770958)) ;
#11512 = CARTESIAN_POINT('',(65.9283765181899,40.85,25.5427692770958)) ;
#11513 = CARTESIAN_POINT('Ctrl Pts',(66.2390177473426,40.85,25.4114596486092)) ;
#11514 = CARTESIAN_POINT('Ctrl Pts',(66.0559344813228,40.85,25.4114596486092)) ;
#11515 = CARTESIAN_POINT('Ctrl Pts',(65.9283765181899,40.85,25.5427692770958)) ;
#11516 = CARTESIAN_POINT('',(65.9283765181899,41.5,25.5427692770958)) ;
#11517 = CARTESIAN_POINT('Ctrl Pts',(66.0259208604693,41.5,26.3486356973648)) ;
#11518 = CARTESIAN_POINT('Ctrl Pts',(66.0259208604693,40.85,26.3486356973648)) ;
#11519 = CARTESIAN_POINT('Ctrl Pts',(66.1324693784118,41.5,26.4154158473015)) ;
#11520 = CARTESIAN_POINT('Ctrl Pts',(66.1324693784118,40.85,26.4154158473015)) ;
#11521 = CARTESIAN_POINT('Ctrl Pts',(66.2495224699378,41.5,26.4154158473015)) ;
#11522 = CARTESIAN_POINT('Ctrl Pts',(66.2495224699378,40.85,26.4154158473015)) ;
#11523 = CARTESIAN_POINT('',(66.0259208604693,40.9767508687437,26.3486356973648)) ;
#11524 = CARTESIAN_POINT('Ctrl Pts',(66.0259208604693,40.9767508687437,26.3486356973648)) ;
#11525 = CARTESIAN_POINT('Ctrl Pts',(66.0600873712772,40.9755766686503,26.370049835812)) ;
#11526 = CARTESIAN_POINT('Ctrl Pts',(66.0964354476884,40.9745939178592,26.3871734830869)) ;
#11527 = CARTESIAN_POINT('Ctrl Pts',(66.1350841335519,40.973923452691,26.3987174084555)) ;
#11528 = CARTESIAN_POINT('Ctrl Pts',(66.1724117020424,40.9732759058487,26.4098667310059)) ;
#11529 = CARTESIAN_POINT('Ctrl Pts',(66.2105599112183,40.9729445751773,26.4154158473015)) ;
#11530 = CARTESIAN_POINT('Ctrl Pts',(66.2495224699378,40.9729445751773,26.4154158473015)) ;
#11531 = CARTESIAN_POINT('',(66.0259208604693,40.85,26.3486356973648)) ;
#11532 = CARTESIAN_POINT('',(66.0259208604693,41.5,26.3486356973648)) ;
#11533 = CARTESIAN_POINT('Ctrl Pts',(66.0259208604693,40.85,26.3486356973648)) ;
#11534 = CARTESIAN_POINT('Ctrl Pts',(66.1324693784118,40.85,26.4154158473015)) ;
#11535 = CARTESIAN_POINT('Ctrl Pts',(66.2495224699378,40.85,26.4154158473015)) ;
#11536 = CARTESIAN_POINT('Ctrl Pts',(65.8600955232978,41.5,26.1542971372604)) ;
#11537 = CARTESIAN_POINT('Ctrl Pts',(65.8600955232978,40.85,26.1542971372604)) ;
#11538 = CARTESIAN_POINT('Ctrl Pts',(65.9193723425269,41.5,26.2818552494049)) ;
#11539 = CARTESIAN_POINT('Ctrl Pts',(65.9193723425269,40.85,26.2818552494049)) ;
#11540 = CARTESIAN_POINT('Ctrl Pts',(66.0259208604693,41.5,26.3486356973648)) ;
#11541 = CARTESIAN_POINT('Ctrl Pts',(66.0259208604693,40.85,26.3486356973648)) ;
#11542 = CARTESIAN_POINT('',(65.8600955232978,40.9861840120855,26.1542971372604)) ;
#11543 = CARTESIAN_POINT('Ctrl Pts',(65.8600955232978,40.9861840120855,26.1542971372604)) ;
#11544 = CARTESIAN_POINT('Ctrl Pts',(65.8788862094647,40.9844755850496,26.1947329177985)) ;
#11545 = CARTESIAN_POINT('Ctrl Pts',(65.9022260091426,40.9827093371832,26.232710898843)) ;
#11546 = CARTESIAN_POINT('Ctrl Pts',(65.9311684027272,40.9810293733619,26.2666352073223)) ;
#11547 = CARTESIAN_POINT('Ctrl Pts',(65.9585896197335,40.9794377063709,26.2987764959093)) ;
#11548 = CARTESIAN_POINT('Ctrl Pts',(65.9901116541869,40.977981528826,26.3261918860119)) ;
#11549 = CARTESIAN_POINT('Ctrl Pts',(66.0259208604693,40.9767508687437,26.3486356973648)) ;
#11550 = CARTESIAN_POINT('',(65.8600955232978,40.85,26.1542971372604)) ;
#11551 = CARTESIAN_POINT('',(65.8600955232978,41.5,26.1542971372604)) ;
#11552 = CARTESIAN_POINT('Ctrl Pts',(65.8600955232978,40.85,26.1542971372604)) ;
#11553 = CARTESIAN_POINT('Ctrl Pts',(65.9193723425269,40.85,26.2818552494049)) ;
#11554 = CARTESIAN_POINT('Ctrl Pts',(66.0259208604693,40.85,26.3486356973648)) ;
#11555 = CARTESIAN_POINT('Ctrl Pts',(65.800818555057,41.5,25.8871759414673)) ;
#11556 = CARTESIAN_POINT('Ctrl Pts',(65.800818555057,40.85,25.8871759414673)) ;
#11557 = CARTESIAN_POINT('Ctrl Pts',(65.800818555057,41.5,26.0267393231392)) ;
#11558 = CARTESIAN_POINT('Ctrl Pts',(65.800818555057,40.85,26.0267393231392)) ;
#11559 = CARTESIAN_POINT('Ctrl Pts',(65.8600955232978,41.5,26.1542971372604)) ;
#11560 = CARTESIAN_POINT('Ctrl Pts',(65.8600955232978,40.85,26.1542971372604)) ;
#11561 = CARTESIAN_POINT('',(65.800818555057,40.995163593533,25.8871759414673)) ;
#11562 = CARTESIAN_POINT('Ctrl Pts',(65.800818555057,40.995163593533,25.8871759414673)) ;
#11563 = CARTESIAN_POINT('Ctrl Pts',(65.800818555057,40.9940128045926,25.9332316514998)) ;
#11564 = CARTESIAN_POINT('Ctrl Pts',(65.8056599512512,40.9926693613796,25.9787682477252)) ;
#11565 = CARTESIAN_POINT('Ctrl Pts',(65.8156338342756,40.9911496437811,26.0237200721573)) ;
#11566 = CARTESIAN_POINT('Ctrl Pts',(65.8256508107933,40.9896233600398,26.068866116949)) ;
#11567 = CARTESIAN_POINT('Ctrl Pts',(65.8406108493885,40.9879555270766,26.1123681640607)) ;
#11568 = CARTESIAN_POINT('Ctrl Pts',(65.8600955232978,40.9861840120855,26.1542971372604)) ;
#11569 = CARTESIAN_POINT('',(65.800818555057,40.85,25.8871759414673)) ;
#11570 = CARTESIAN_POINT('',(65.800818555057,41.5,25.8871759414673)) ;
#11571 = CARTESIAN_POINT('Ctrl Pts',(65.800818555057,40.85,25.8871759414673)) ;
#11572 = CARTESIAN_POINT('Ctrl Pts',(65.800818555057,40.85,26.0267393231392)) ;
#11573 = CARTESIAN_POINT('Ctrl Pts',(65.8600955232978,40.85,26.1542971372604)) ;
#11574 = CARTESIAN_POINT('Ctrl Pts',(65.9283765181899,41.5,25.5427692770958)) ;
#11575 = CARTESIAN_POINT('Ctrl Pts',(65.9283765181899,40.85,25.5427692770958)) ;
#11576 = CARTESIAN_POINT('Ctrl Pts',(65.800818555057,41.5,25.6740789055824)) ;
#11577 = CARTESIAN_POINT('Ctrl Pts',(65.800818555057,40.85,25.6740789055824)) ;
#11578 = CARTESIAN_POINT('Ctrl Pts',(65.800818555057,41.5,25.8871759414673)) ;
#11579 = CARTESIAN_POINT('Ctrl Pts',(65.800818555057,40.85,25.8871759414673)) ;
#11580 = CARTESIAN_POINT('Ctrl Pts',(65.9283765181899,40.9999409930792,25.5427692770958)) ;
#11581 = CARTESIAN_POINT('Ctrl Pts',(65.8879994387808,40.9998263030235,25.5843339051784)) ;
#11582 = CARTESIAN_POINT('Ctrl Pts',(65.8571868924283,40.9995311591319,25.63206654485)) ;
#11583 = CARTESIAN_POINT('Ctrl Pts',(65.8359691306507,40.998884127952,25.6859859895723)) ;
#11584 = CARTESIAN_POINT('Ctrl Pts',(65.8107777994687,40.9981159236094,25.7500032315125)) ;
#11585 = CARTESIAN_POINT('Ctrl Pts',(65.800818555057,40.9968816429754,25.8184179058545)) ;
#11586 = CARTESIAN_POINT('Ctrl Pts',(65.800818555057,40.995163593533,25.8871759414673)) ;
#11587 = CARTESIAN_POINT('Ctrl Pts',(65.9283765181899,40.85,25.5427692770958)) ;
#11588 = CARTESIAN_POINT('Ctrl Pts',(65.800818555057,40.85,25.6740789055824)) ;
#11589 = CARTESIAN_POINT('Ctrl Pts',(65.800818555057,40.85,25.8871759414673)) ;
#11590 = CARTESIAN_POINT('Ctrl Pts',(66.2795360907912,41.5,24.3909957945347)) ;
#11591 = CARTESIAN_POINT('Ctrl Pts',(66.2795360907912,40.85,24.3909957945347)) ;
#11592 = CARTESIAN_POINT('Ctrl Pts',(66.5391542539001,41.5,24.3909957945347)) ;
#11593 = CARTESIAN_POINT('Ctrl Pts',(66.5391542539001,40.85,24.3909957945347)) ;
#11594 = CARTESIAN_POINT('Ctrl Pts',(66.70497944206,41.5,24.5365619599819)) ;
#11595 = CARTESIAN_POINT('Ctrl Pts',(66.70497944206,40.85,24.5365619599819)) ;
#11596 = CARTESIAN_POINT('',(66.70497944206,40.9700286729872,24.5365619599819)) ;
#11597 = CARTESIAN_POINT('Ctrl Pts',(66.2795360907912,40.9602752133414,24.3909957945347)) ;
#11598 = CARTESIAN_POINT('Ctrl Pts',(66.3597536157927,40.9602752133414,24.3909957945347)) ;
#11599 = CARTESIAN_POINT('Ctrl Pts',(66.4398014503548,40.9610411641504,24.4014174188477)) ;
#11600 = CARTESIAN_POINT('Ctrl Pts',(66.51569958686,40.9628424734339,24.427385138193)) ;
#11601 = CARTESIAN_POINT('Ctrl Pts',(66.5859662839039,40.964510130369,24.4514261219665)) ;
#11602 = CARTESIAN_POINT('Ctrl Pts',(66.6492016541882,40.9669793466799,24.4875985980963)) ;
#11603 = CARTESIAN_POINT('Ctrl Pts',(66.70497944206,40.9700286729872,24.5365619599819)) ;
#11604 = CARTESIAN_POINT('',(66.70497944206,40.85,24.5365619599819)) ;
#11605 = CARTESIAN_POINT('Ctrl Pts',(66.2795360907912,40.85,24.3909957945347)) ;
#11606 = CARTESIAN_POINT('Ctrl Pts',(66.5391542539001,40.85,24.3909957945347)) ;
#11607 = CARTESIAN_POINT('Ctrl Pts',(66.70497944206,40.85,24.5365619599819)) ;
#11608 = CARTESIAN_POINT('',(66.70497944206,41.5,24.5365619599819)) ;
#11609 = CARTESIAN_POINT('Ctrl Pts',(65.9974079355597,41.5,25.2448838889599)) ;
#11610 = CARTESIAN_POINT('Ctrl Pts',(65.9974079355597,40.85,25.2448838889599)) ;
#11611 = CARTESIAN_POINT('Ctrl Pts',(66.1384720131755,41.5,25.172851228714)) ;
#11612 = CARTESIAN_POINT('Ctrl Pts',(66.1384720131755,40.85,25.172851228714)) ;
#11613 = CARTESIAN_POINT('Ctrl Pts',(66.2930422052741,41.5,25.172851228714)) ;
#11614 = CARTESIAN_POINT('Ctrl Pts',(66.2930422052741,40.85,25.172851228714)) ;
#11615 = CARTESIAN_POINT('',(65.9974079355597,40.9979003664976,25.2448838889599)) ;
#11616 = CARTESIAN_POINT('Ctrl Pts',(65.9974079355597,40.9979003664976,25.2448838889599)) ;
#11617 = CARTESIAN_POINT('Ctrl Pts',(66.0434771360032,40.9975131189137,25.2213592105341)) ;
#11618 = CARTESIAN_POINT('Ctrl Pts',(66.0915879306606,40.9971611542325,25.2031057712063)) ;
#11619 = CARTESIAN_POINT('Ctrl Pts',(66.1418468502283,40.9969168656354,25.1908598059363)) ;
#11620 = CARTESIAN_POINT('Ctrl Pts',(66.1915089745217,40.9966754778225,25.1787592543414)) ;
#11621 = CARTESIAN_POINT('Ctrl Pts',(66.2419264991158,40.9965471535257,25.172851228714)) ;
#11622 = CARTESIAN_POINT('Ctrl Pts',(66.2930422052741,40.9965471535257,25.172851228714)) ;
#11623 = CARTESIAN_POINT('',(65.9974079355597,40.85,25.2448838889599)) ;
#11624 = CARTESIAN_POINT('',(65.9974079355597,41.5,25.2448838889599)) ;
#11625 = CARTESIAN_POINT('Ctrl Pts',(65.9974079355597,40.85,25.2448838889599)) ;
#11626 = CARTESIAN_POINT('Ctrl Pts',(66.1384720131755,40.85,25.172851228714)) ;
#11627 = CARTESIAN_POINT('Ctrl Pts',(66.2930422052741,40.85,25.172851228714)) ;
#11628 = CARTESIAN_POINT('Ctrl Pts',(65.758799366653,41.5,25.4654841065407)) ;
#11629 = CARTESIAN_POINT('Ctrl Pts',(65.758799366653,40.85,25.4654841065407)) ;
#11630 = CARTESIAN_POINT('Ctrl Pts',(65.8563437089324,41.5,25.3169166982174)) ;
#11631 = CARTESIAN_POINT('Ctrl Pts',(65.8563437089324,40.85,25.3169166982174)) ;
#11632 = CARTESIAN_POINT('Ctrl Pts',(65.9974079355597,41.5,25.2448838889599)) ;
#11633 = CARTESIAN_POINT('Ctrl Pts',(65.9974079355597,40.85,25.2448838889599)) ;
#11634 = CARTESIAN_POINT('',(65.758799366653,40.9999615694072,25.4654841065407)) ;
#11635 = CARTESIAN_POINT('Ctrl Pts',(65.758799366653,40.9999615694072,25.4654841065407)) ;
#11636 = CARTESIAN_POINT('Ctrl Pts',(65.7898404317904,40.9998562892375,25.4182062174156)) ;
#11637 = CARTESIAN_POINT('Ctrl Pts',(65.8256934781911,40.9995390458235,25.3744462358198)) ;
#11638 = CARTESIAN_POINT('Ctrl Pts',(65.8672232792857,40.9991328993943,25.3360507184735)) ;
#11639 = CARTESIAN_POINT('Ctrl Pts',(65.9064830807812,40.9987489527399,25.2997538822354)) ;
#11640 = CARTESIAN_POINT('Ctrl Pts',(65.949789164042,40.998300639841,25.2691998616755)) ;
#11641 = CARTESIAN_POINT('Ctrl Pts',(65.9974079355597,40.9979003664976,25.2448838889599)) ;
#11642 = CARTESIAN_POINT('',(65.758799366653,40.85,25.4654841065407)) ;
#11643 = CARTESIAN_POINT('',(65.758799366653,41.5,25.4654841065407)) ;
#11644 = CARTESIAN_POINT('Ctrl Pts',(65.758799366653,40.85,25.4654841065407)) ;
#11645 = CARTESIAN_POINT('Ctrl Pts',(65.8563437089324,40.85,25.3169166982174)) ;
#11646 = CARTESIAN_POINT('Ctrl Pts',(65.9974079355597,40.85,25.2448838889599)) ;
#11647 = CARTESIAN_POINT('Ctrl Pts',(65.835334263742,41.5,24.9567529499531)) ;
#11648 = CARTESIAN_POINT('Ctrl Pts',(65.835334263742,40.85,24.9567529499531)) ;
#11649 = CARTESIAN_POINT('Ctrl Pts',(65.7618007585406,41.5,25.1353341281414)) ;
#11650 = CARTESIAN_POINT('Ctrl Pts',(65.7618007585406,40.85,25.1353341281414)) ;
#11651 = CARTESIAN_POINT('Ctrl Pts',(65.758799366653,41.5,25.4654841065407)) ;
#11652 = CARTESIAN_POINT('Ctrl Pts',(65.758799366653,40.85,25.4654841065407)) ;
#11653 = CARTESIAN_POINT('',(65.835334263742,40.9904771599398,24.9567529499531)) ;
#11654 = CARTESIAN_POINT('Ctrl Pts',(65.835334263742,40.9904771599398,24.9567529499531)) ;
#11655 = CARTESIAN_POINT('Ctrl Pts',(65.8204030637459,40.9917488395531,24.9930143967556)) ;
#11656 = CARTESIAN_POINT('Ctrl Pts',(65.8085450275128,40.9929650207556,25.0318073588892)) ;
#11657 = CARTESIAN_POINT('Ctrl Pts',(65.7990827857526,40.9940545364855,25.0711309699265)) ;
#11658 = CARTESIAN_POINT('Ctrl Pts',(65.7908915214191,40.9949977074132,25.1051725956554)) ;
#11659 = CARTESIAN_POINT('Ctrl Pts',(65.7844937127903,40.9958459552111,25.1396076926084)) ;
#11660 = CARTESIAN_POINT('Ctrl Pts',(65.7794477485054,40.9965531109567,25.1731335451618)) ;
#11661 = CARTESIAN_POINT('Ctrl Pts',(65.7697518635822,40.9979119197681,25.2375538997173)) ;
#11662 = CARTESIAN_POINT('Ctrl Pts',(65.7641154541389,40.9988966859177,25.3048486747571)) ;
#11663 = CARTESIAN_POINT('Ctrl Pts',(65.7612165577635,40.9994566523273,25.3714502213717)) ;
#11664 = CARTESIAN_POINT('Ctrl Pts',(65.7598399751179,40.9997225604323,25.4030769238695)) ;
#11665 = CARTESIAN_POINT('Ctrl Pts',(65.7590806144596,40.9998926778167,25.4345471410405)) ;
#11666 = CARTESIAN_POINT('Ctrl Pts',(65.758799366653,40.9999615694072,25.4654841065407)) ;
#11667 = CARTESIAN_POINT('',(65.835334263742,40.85,24.9567529499531)) ;
#11668 = CARTESIAN_POINT('',(65.835334263742,41.5,24.9567529499531)) ;
#11669 = CARTESIAN_POINT('Ctrl Pts',(65.835334263742,40.85,24.9567529499531)) ;
#11670 = CARTESIAN_POINT('Ctrl Pts',(65.7618007585406,40.85,25.1353341281414)) ;
#11671 = CARTESIAN_POINT('Ctrl Pts',(65.758799366653,40.85,25.4654841065407)) ;
#11672 = CARTESIAN_POINT('Ctrl Pts',(66.0364255830646,41.5,24.6851295173168)) ;
#11673 = CARTESIAN_POINT('Ctrl Pts',(66.0364255830646,40.85,24.6851295173168)) ;
#11674 = CARTESIAN_POINT('Ctrl Pts',(65.9088676199317,41.5,24.7781717717648)) ;
#11675 = CARTESIAN_POINT('Ctrl Pts',(65.9088676199317,40.85,24.7781717717648)) ;
#11676 = CARTESIAN_POINT('Ctrl Pts',(65.835334263742,41.5,24.9567529499531)) ;
#11677 = CARTESIAN_POINT('Ctrl Pts',(65.835334263742,40.85,24.9567529499531)) ;
#11678 = CARTESIAN_POINT('',(66.0364255830646,40.9785653759143,24.6851295173168)) ;
#11679 = CARTESIAN_POINT('Ctrl Pts',(66.0364255830646,40.9785653759143,24.6851295173168)) ;
#11680 = CARTESIAN_POINT('Ctrl Pts',(65.9924837093702,40.9802527411659,24.717181228498)) ;
#11681 = CARTESIAN_POINT('Ctrl Pts',(65.9547589853903,40.9821868075603,24.7558189502039)) ;
#11682 = CARTESIAN_POINT('Ctrl Pts',(65.922400046105,40.9841638195929,24.7995210152964)) ;
#11683 = CARTESIAN_POINT('Ctrl Pts',(65.8866774648815,40.9863463377616,24.8477658157868)) ;
#11684 = CARTESIAN_POINT('Ctrl Pts',(65.8581900211715,40.9885305474988,24.9012460575488)) ;
#11685 = CARTESIAN_POINT('Ctrl Pts',(65.835334263742,40.9904771599398,24.9567529499531)) ;
#11686 = CARTESIAN_POINT('',(66.0364255830646,40.85,24.6851295173168)) ;
#11687 = CARTESIAN_POINT('',(66.0364255830646,41.5,24.6851295173168)) ;
#11688 = CARTESIAN_POINT('Ctrl Pts',(66.0364255830646,40.85,24.6851295173168)) ;
#11689 = CARTESIAN_POINT('Ctrl Pts',(65.9088676199317,40.85,24.7781717717648)) ;
#11690 = CARTESIAN_POINT('Ctrl Pts',(65.835334263742,40.85,24.9567529499531)) ;
#11691 = CARTESIAN_POINT('Ctrl Pts',(66.2630285844207,41.5,24.6130967080593)) ;
#11692 = CARTESIAN_POINT('Ctrl Pts',(66.2630285844207,40.85,24.6130967080593)) ;
#11693 = CARTESIAN_POINT('Ctrl Pts',(66.133969925344,41.5,24.6130967080593)) ;
#11694 = CARTESIAN_POINT('Ctrl Pts',(66.133969925344,40.85,24.6130967080593)) ;
#11695 = CARTESIAN_POINT('Ctrl Pts',(66.0364255830646,41.5,24.6851295173168)) ;
#11696 = CARTESIAN_POINT('Ctrl Pts',(66.0364255830646,40.85,24.6851295173168)) ;
#11697 = CARTESIAN_POINT('',(66.2630285844207,40.9746050854535,24.6130967080593)) ;
#11698 = CARTESIAN_POINT('Ctrl Pts',(66.2630285844207,40.9746050854535,24.6130967080593)) ;
#11699 = CARTESIAN_POINT('Ctrl Pts',(66.2217889884937,40.9746050854535,24.6130967080593)) ;
#11700 = CARTESIAN_POINT('Ctrl Pts',(66.1811469291785,40.9749253007144,24.618612753171)) ;
#11701 = CARTESIAN_POINT('Ctrl Pts',(66.1418490530652,40.975626676171,24.6311047360094)) ;
#11702 = CARTESIAN_POINT('Ctrl Pts',(66.1037031127777,40.9763074922591,24.6432305422503)) ;
#11703 = CARTESIAN_POINT('Ctrl Pts',(66.0686131950993,40.9773140371269,24.661360182633)) ;
#11704 = CARTESIAN_POINT('Ctrl Pts',(66.0364255830646,40.9785653759143,24.6851295173168)) ;
#11705 = CARTESIAN_POINT('',(66.2630285844207,40.85,24.6130967080593)) ;
#11706 = CARTESIAN_POINT('',(66.2630285844207,41.5,24.6130967080593)) ;
#11707 = CARTESIAN_POINT('Ctrl Pts',(66.2630285844207,40.85,24.6130967080593)) ;
#11708 = CARTESIAN_POINT('Ctrl Pts',(66.133969925344,40.85,24.6130967080593)) ;
#11709 = CARTESIAN_POINT('Ctrl Pts',(66.0364255830646,40.85,24.6851295173168)) ;
#11710 = CARTESIAN_POINT('Ctrl Pts',(66.5331514701247,41.5,24.7286492526531)) ;
#11711 = CARTESIAN_POINT('Ctrl Pts',(66.5331514701247,40.85,24.7286492526531)) ;
#11712 = CARTESIAN_POINT('Ctrl Pts',(66.4236017093062,41.5,24.6130967080593)) ;
#11713 = CARTESIAN_POINT('Ctrl Pts',(66.4236017093062,40.85,24.6130967080593)) ;
#11714 = CARTESIAN_POINT('Ctrl Pts',(66.2630285844207,41.5,24.6130967080593)) ;
#11715 = CARTESIAN_POINT('Ctrl Pts',(66.2630285844207,40.85,24.6130967080593)) ;
#11716 = CARTESIAN_POINT('',(66.5331514701247,40.9807951354111,24.7286492526531)) ;
#11717 = CARTESIAN_POINT('Ctrl Pts',(66.5331514701247,40.9807951354111,24.7286492526531)) ;
#11718 = CARTESIAN_POINT('Ctrl Pts',(66.4991519463673,40.9790082382666,24.6927867235541)) ;
#11719 = CARTESIAN_POINT('Ctrl Pts',(66.4599857285765,40.9774358576459,24.6637099460066)) ;
#11720 = CARTESIAN_POINT('Ctrl Pts',(66.4147776930977,40.9763284909537,24.6436960585779)) ;
#11721 = CARTESIAN_POINT('Ctrl Pts',(66.3914684127497,40.9757575322645,24.6333768905808)) ;
#11722 = CARTESIAN_POINT('Ctrl Pts',(66.3672753064892,40.9753279903153,24.6257865971459)) ;
#11723 = CARTESIAN_POINT('Ctrl Pts',(66.3422822541488,40.9750416415541,24.6207467986028)) ;
#11724 = CARTESIAN_POINT('Ctrl Pts',(66.3161714606551,40.9747424866822,24.615481609813)) ;
#11725 = CARTESIAN_POINT('Ctrl Pts',(66.2896659598749,40.9746050854535,24.6130967080593)) ;
#11726 = CARTESIAN_POINT('Ctrl Pts',(66.2630285844207,40.9746050854535,24.6130967080593)) ;
#11727 = CARTESIAN_POINT('',(66.5331514701247,40.85,24.7286492526531)) ;
#11728 = CARTESIAN_POINT('',(66.5331514701247,41.5,24.7286492526531)) ;
#11729 = CARTESIAN_POINT('Ctrl Pts',(66.5331514701247,40.85,24.7286492526531)) ;
#11730 = CARTESIAN_POINT('Ctrl Pts',(66.4236017093062,40.85,24.6130967080593)) ;
#11731 = CARTESIAN_POINT('Ctrl Pts',(66.2630285844207,40.85,24.6130967080593)) ;
#11732 = CARTESIAN_POINT('Ctrl Pts',(66.6351976022124,41.5,24.9597543418407)) ;
#11733 = CARTESIAN_POINT('Ctrl Pts',(66.6351976022124,40.85,24.9597543418407)) ;
#11734 = CARTESIAN_POINT('Ctrl Pts',(66.5991814956069,41.5,24.8006820619106)) ;
#11735 = CARTESIAN_POINT('Ctrl Pts',(66.5991814956069,40.85,24.8006820619106)) ;
#11736 = CARTESIAN_POINT('Ctrl Pts',(66.5331514701247,41.5,24.7286492526531)) ;
#11737 = CARTESIAN_POINT('Ctrl Pts',(66.5331514701247,40.85,24.7286492526531)) ;
#11738 = CARTESIAN_POINT('',(66.6351976022124,40.990582126855,24.9597543418407)) ;
#11739 = CARTESIAN_POINT('Ctrl Pts',(66.6351976022124,40.990582126855,24.9597543418407)) ;
#11740 = CARTESIAN_POINT('Ctrl Pts',(66.6255826971324,40.9891010885524,24.9172882060882)) ;
#11741 = CARTESIAN_POINT('Ctrl Pts',(66.6129385031804,40.987370907003,24.8731722925374)) ;
#11742 = CARTESIAN_POINT('Ctrl Pts',(66.5960584064866,40.9856269527389,24.8326553272909)) ;
#11743 = CARTESIAN_POINT('Ctrl Pts',(66.5946335153935,40.9854797412068,24.8292351891278)) ;
#11744 = CARTESIAN_POINT('Ctrl Pts',(66.5931784586585,40.9853324315375,24.8258406454158)) ;
#11745 = CARTESIAN_POINT('Ctrl Pts',(66.5916925287781,40.9851851653016,24.8224748002298)) ;
#11746 = CARTESIAN_POINT('Ctrl Pts',(66.579173590795,40.9839444493707,24.7941176026917)) ;
#11747 = CARTESIAN_POINT('Ctrl Pts',(66.5635747988376,40.9826176783275,24.7657800092439)) ;
#11748 = CARTESIAN_POINT('Ctrl Pts',(66.5440341374292,40.9814230256515,24.7413666657469)) ;
#11749 = CARTESIAN_POINT('Ctrl Pts',(66.5405345731193,40.9812090736373,24.7369944460047)) ;
#11750 = CARTESIAN_POINT('Ctrl Pts',(66.5369086215402,40.9809993591517,24.7327479663714)) ;
#11751 = CARTESIAN_POINT('Ctrl Pts',(66.5331514701247,40.9807951354111,24.7286492526531)) ;
#11752 = CARTESIAN_POINT('',(66.6351976022124,40.85,24.9597543418407)) ;
#11753 = CARTESIAN_POINT('',(66.6351976022124,41.5,24.9597543418407)) ;
#11754 = CARTESIAN_POINT('Ctrl Pts',(66.6351976022124,40.85,24.9597543418407)) ;
#11755 = CARTESIAN_POINT('Ctrl Pts',(66.5991814956069,40.85,24.8006820619106)) ;
#11756 = CARTESIAN_POINT('Ctrl Pts',(66.5331514701247,40.85,24.7286492526531)) ;
#11757 = CARTESIAN_POINT('Origin',(66.9038199409842,41.5,24.9387447476387)) ;
#11758 = CARTESIAN_POINT('',(66.9038199409842,40.9898351360399,24.9387447476387)) ;
#11759 = CARTESIAN_POINT('Origin',(59.7277794574127,25.5,25.5)) ;
#11760 = CARTESIAN_POINT('',(66.9038199409842,40.85,24.9387447476387)) ;
#11761 = CARTESIAN_POINT('',(66.9038199409842,41.5,24.9387447476387)) ;
#11762 = CARTESIAN_POINT('',(66.9038199409842,40.85,24.9387447476387)) ;
#11763 = CARTESIAN_POINT('Ctrl Pts',(66.70497944206,41.5,24.5365619599819)) ;
#11764 = CARTESIAN_POINT('Ctrl Pts',(66.70497944206,40.85,24.5365619599819)) ;
#11765 = CARTESIAN_POINT('Ctrl Pts',(66.8708049282432,41.5,24.6821281254292)) ;
#11766 = CARTESIAN_POINT('Ctrl Pts',(66.8708049282432,40.85,24.6821281254292)) ;
#11767 = CARTESIAN_POINT('Ctrl Pts',(66.9038199409842,41.5,24.9387447476387)) ;
#11768 = CARTESIAN_POINT('Ctrl Pts',(66.9038199409842,40.85,24.9387447476387)) ;
#11769 = CARTESIAN_POINT('Ctrl Pts',(66.70497944206,40.9700286729872,24.5365619599819)) ;
#11770 = CARTESIAN_POINT('Ctrl Pts',(66.7606666603835,40.9730730424596,24.5854457294335)) ;
#11771 = CARTESIAN_POINT('Ctrl Pts',(66.8046639769613,40.9764505641981,24.6433213282491)) ;
#11772 = CARTESIAN_POINT('Ctrl Pts',(66.8375183760913,40.9798404114639,24.7097210393724)) ;
#11773 = CARTESIAN_POINT('Ctrl Pts',(66.8730210352428,40.9835035005855,24.781472962226)) ;
#11774 = CARTESIAN_POINT('Ctrl Pts',(66.8936025795082,40.9869575673714,24.8593280044003)) ;
#11775 = CARTESIAN_POINT('Ctrl Pts',(66.9038199409842,40.9898351360399,24.9387447476387)) ;
#11776 = CARTESIAN_POINT('Ctrl Pts',(66.70497944206,40.85,24.5365619599819)) ;
#11777 = CARTESIAN_POINT('Ctrl Pts',(66.8708049282432,40.85,24.6821281254292)) ;
#11778 = CARTESIAN_POINT('Ctrl Pts',(66.9038199409842,40.85,24.9387447476387)) ;
#11779 = CARTESIAN_POINT('Origin',(65.4714187197387,40.85,25.5142562776804)) ;
#11780 = CARTESIAN_POINT('Ctrl Pts',(64.2843792364001,41.5,25.0648020148277)) ;
#11781 = CARTESIAN_POINT('Ctrl Pts',(64.2843792364001,40.85,25.0648020148277)) ;
#11782 = CARTESIAN_POINT('Ctrl Pts',(64.1260573044419,41.5,25.1578442692757)) ;
#11783 = CARTESIAN_POINT('Ctrl Pts',(64.1260573044419,40.85,25.1578442692757)) ;
#11784 = CARTESIAN_POINT('Ctrl Pts',(64.,41.5,25.2043653964996)) ;
#11785 = CARTESIAN_POINT('Ctrl Pts',(64.,40.85,25.2043653964996)) ;
#11786 = CARTESIAN_POINT('',(64.2843792364001,40.9938892055449,25.0648020148277)) ;
#11787 = CARTESIAN_POINT('',(64.,40.9971803945496,25.2043653964996)) ;
#11788 = CARTESIAN_POINT('Ctrl Pts',(64.2843792364001,40.9938892055449,25.0648020148277)) ;
#11789 = CARTESIAN_POINT('Ctrl Pts',(64.2355786561281,40.9946947519433,25.0934810231668)) ;
#11790 = CARTESIAN_POINT('Ctrl Pts',(64.1849598543689,40.9953922950403,25.1212649766542)) ;
#11791 = CARTESIAN_POINT('Ctrl Pts',(64.1341309103538,40.9959618246374,25.1462103317239)) ;
#11792 = CARTESIAN_POINT('Ctrl Pts',(64.0907067039323,40.9964483854203,25.1675216587403)) ;
#11793 = CARTESIAN_POINT('Ctrl Pts',(64.0453985127022,40.9968607800921,25.1876111909853)) ;
#11794 = CARTESIAN_POINT('Ctrl Pts',(64.,40.9971803945496,25.2043653964996)) ;
#11795 = CARTESIAN_POINT('',(64.2843792364001,40.85,25.0648020148277)) ;
#11796 = CARTESIAN_POINT('',(64.2843792364001,41.5,25.0648020148277)) ;
#11797 = CARTESIAN_POINT('',(64.,40.85,25.2043653964996)) ;
#11798 = CARTESIAN_POINT('Ctrl Pts',(64.2843792364001,40.85,25.0648020148277)) ;
#11799 = CARTESIAN_POINT('Ctrl Pts',(64.1260573044419,40.85,25.1578442692757)) ;
#11800 = CARTESIAN_POINT('Ctrl Pts',(64.,40.85,25.2043653964996)) ;
#11801 = CARTESIAN_POINT('',(64.,41.5,25.2043653964996)) ;
#11802 = CARTESIAN_POINT('Origin',(64.,41.5,25.2043653964996)) ;
#11803 = CARTESIAN_POINT('',(64.,40.9899976032232,24.9432466864586)) ;
#11804 = CARTESIAN_POINT('Origin',(64.,25.5,25.5)) ;
#11805 = CARTESIAN_POINT('',(64.,40.85,24.9432466864586)) ;
#11806 = CARTESIAN_POINT('',(64.,40.85,25.2043653964996)) ;
#11807 = CARTESIAN_POINT('',(64.,41.5,24.9432466864586)) ;
#11808 = CARTESIAN_POINT('Ctrl Pts',(64.,41.5,24.9432466864586)) ;
#11809 = CARTESIAN_POINT('Ctrl Pts',(64.,40.85,24.9432466864586)) ;
#11810 = CARTESIAN_POINT('Ctrl Pts',(64.2266030013561,41.5,24.8366983175278)) ;
#11811 = CARTESIAN_POINT('Ctrl Pts',(64.2266030013561,40.85,24.8366983175278)) ;
#11812 = CARTESIAN_POINT('Ctrl Pts',(64.3961801156402,41.5,24.6851293683052)) ;
#11813 = CARTESIAN_POINT('Ctrl Pts',(64.3961801156402,40.85,24.6851293683052)) ;
#11814 = CARTESIAN_POINT('',(64.3961801156402,40.9785653680695,24.6851293683052)) ;
#11815 = CARTESIAN_POINT('Ctrl Pts',(64.,40.9899976032232,24.9432466864586)) ;
#11816 = CARTESIAN_POINT('Ctrl Pts',(64.0733426948616,40.9887580948318,24.9087610685995)) ;
#11817 = CARTESIAN_POINT('Ctrl Pts',(64.1444161728547,40.9872424953141,24.8696983737347)) ;
#11818 = CARTESIAN_POINT('Ctrl Pts',(64.2123120711965,40.9853157337165,24.8254656219949)) ;
#11819 = CARTESIAN_POINT('Ctrl Pts',(64.2770804763103,40.9834777246651,24.7832703664057)) ;
#11820 = CARTESIAN_POINT('Ctrl Pts',(64.3385649661852,40.9812764188499,24.7366261029859)) ;
#11821 = CARTESIAN_POINT('Ctrl Pts',(64.3961801156402,40.9785653680695,24.6851293683052)) ;
#11822 = CARTESIAN_POINT('',(64.3961801156402,40.85,24.6851293683052)) ;
#11823 = CARTESIAN_POINT('Ctrl Pts',(64.,40.85,24.9432466864586)) ;
#11824 = CARTESIAN_POINT('Ctrl Pts',(64.2266030013561,40.85,24.8366983175278)) ;
#11825 = CARTESIAN_POINT('Ctrl Pts',(64.3961801156402,40.85,24.6851293683052)) ;
#11826 = CARTESIAN_POINT('',(64.3961801156402,41.5,24.6851293683052)) ;
#11827 = CARTESIAN_POINT('Ctrl Pts',(64.3961801156402,41.5,24.6851293683052)) ;
#11828 = CARTESIAN_POINT('Ctrl Pts',(64.3961801156402,40.85,24.6851293683052)) ;
#11829 = CARTESIAN_POINT('Ctrl Pts',(64.5657571181655,41.5,24.5335605680943)) ;
#11830 = CARTESIAN_POINT('Ctrl Pts',(64.5657571181655,40.85,24.5335605680943)) ;
#11831 = CARTESIAN_POINT('Ctrl Pts',(64.6362892314792,41.5,24.3909957945347)) ;
#11832 = CARTESIAN_POINT('Ctrl Pts',(64.6362892314792,40.85,24.3909957945347)) ;
#11833 = CARTESIAN_POINT('',(64.6362892314792,40.9602752133414,24.3909957945347)) ;
#11834 = CARTESIAN_POINT('Ctrl Pts',(64.3961801156402,40.9785653680695,24.6851293683052)) ;
#11835 = CARTESIAN_POINT('Ctrl Pts',(64.4474761123885,40.9761516625032,24.6392807416224)) ;
#11836 = CARTESIAN_POINT('Ctrl Pts',(64.4974059529476,40.9733088517611,24.5891960070225)) ;
#11837 = CARTESIAN_POINT('Ctrl Pts',(64.5409178996485,40.969987876403,24.5359071082398)) ;
#11838 = CARTESIAN_POINT('Ctrl Pts',(64.5773705983453,40.9672056861476,24.491263640905)) ;
#11839 = CARTESIAN_POINT('Ctrl Pts',(64.6107423855321,40.9639792782932,24.4426329869638)) ;
#11840 = CARTESIAN_POINT('Ctrl Pts',(64.6362892314792,40.9602752133414,24.3909957945347)) ;
#11841 = CARTESIAN_POINT('',(64.6362892314792,40.85,24.3909957945347)) ;
#11842 = CARTESIAN_POINT('Ctrl Pts',(64.3961801156402,40.85,24.6851293683052)) ;
#11843 = CARTESIAN_POINT('Ctrl Pts',(64.5657571181655,40.85,24.5335605680943)) ;
#11844 = CARTESIAN_POINT('Ctrl Pts',(64.6362892314792,40.85,24.3909957945347)) ;
#11845 = CARTESIAN_POINT('',(64.6362892314792,41.5,24.3909957945347)) ;
#11846 = CARTESIAN_POINT('Origin',(64.6362892314792,41.5,24.3909957945347)) ;
#11847 = CARTESIAN_POINT('',(64.810368321836,40.9602752133414,24.3909957945347)) ;
#11848 = CARTESIAN_POINT('',(55.25,40.9602752133414,24.3909957945347)) ;
#11849 = CARTESIAN_POINT('',(64.810368321836,40.85,24.3909957945347)) ;
#11850 = CARTESIAN_POINT('',(64.6362892314792,40.85,24.3909957945347)) ;
#11851 = CARTESIAN_POINT('',(64.810368321836,41.5,24.3909957945347)) ;
#11852 = CARTESIAN_POINT('Ctrl Pts',(64.5402455851436,41.5,24.8787173569202)) ;
#11853 = CARTESIAN_POINT('Ctrl Pts',(64.5402455851436,40.85,24.8787173569202)) ;
#11854 = CARTESIAN_POINT('Ctrl Pts',(64.4427012428641,41.5,24.9717597603798)) ;
#11855 = CARTESIAN_POINT('Ctrl Pts',(64.4427012428641,40.85,24.9717597603798)) ;
#11856 = CARTESIAN_POINT('Ctrl Pts',(64.2843792364001,41.5,25.0648020148277)) ;
#11857 = CARTESIAN_POINT('Ctrl Pts',(64.2843792364001,40.85,25.0648020148277)) ;
#11858 = CARTESIAN_POINT('',(64.5402455851436,40.987543636013,24.8787173569202)) ;
#11859 = CARTESIAN_POINT('Ctrl Pts',(64.5402455851436,40.987543636013,24.8787173569202)) ;
#11860 = CARTESIAN_POINT('Ctrl Pts',(64.5051954022992,40.9888847812188,24.9121498777342)) ;
#11861 = CARTESIAN_POINT('Ctrl Pts',(64.4666886720027,40.9900244116147,24.9432630014271)) ;
#11862 = CARTESIAN_POINT('Ctrl Pts',(64.4275224800183,40.9909957776269,24.9717483388133)) ;
#11863 = CARTESIAN_POINT('Ctrl Pts',(64.381760456328,40.9921307277512,25.0050307851846)) ;
#11864 = CARTESIAN_POINT('Ctrl Pts',(64.3331543424579,40.9930840800258,25.0361379906033)) ;
#11865 = CARTESIAN_POINT('Ctrl Pts',(64.2843792364001,40.9938892055449,25.0648020148277)) ;
#11866 = CARTESIAN_POINT('',(64.5402455851436,40.85,24.8787173569202)) ;
#11867 = CARTESIAN_POINT('',(64.5402455851436,41.5,24.8787173569202)) ;
#11868 = CARTESIAN_POINT('Ctrl Pts',(64.5402455851436,40.85,24.8787173569202)) ;
#11869 = CARTESIAN_POINT('Ctrl Pts',(64.4427012428641,40.85,24.9717597603798)) ;
#11870 = CARTESIAN_POINT('Ctrl Pts',(64.2843792364001,40.85,25.0648020148277)) ;
#11871 = CARTESIAN_POINT('Origin',(64.5402455851436,41.5,26.5999998092651)) ;
#11872 = CARTESIAN_POINT('',(64.5402455851436,40.9609184856404,26.5999998092651)) ;
#11873 = CARTESIAN_POINT('Origin',(64.5402455851436,25.5,25.5)) ;
#11874 = CARTESIAN_POINT('',(64.5402455851436,40.85,26.5999998092651)) ;
#11875 = CARTESIAN_POINT('',(64.5402455851436,41.5,26.5999998092651)) ;
#11876 = CARTESIAN_POINT('',(64.5402455851436,40.85,26.5999998092651)) ;
#11877 = CARTESIAN_POINT('Origin',(64.810368321836,41.5,26.5999998092651)) ;
#11878 = CARTESIAN_POINT('',(64.810368321836,40.9609184856404,26.5999998092651)) ;
#11879 = CARTESIAN_POINT('',(55.25,40.9609184856404,26.5999998092651)) ;
#11880 = CARTESIAN_POINT('',(64.810368321836,40.85,26.5999998092651)) ;
#11881 = CARTESIAN_POINT('',(64.810368321836,41.5,26.5999998092651)) ;
#11882 = CARTESIAN_POINT('',(64.810368321836,40.85,26.5999998092651)) ;
#11883 = CARTESIAN_POINT('Origin',(64.810368321836,41.5,24.3909957945347)) ;
#11884 = CARTESIAN_POINT('Origin',(64.810368321836,25.5,25.5)) ;
#11885 = CARTESIAN_POINT('',(64.810368321836,40.85,24.3909957945347)) ;
#11886 = CARTESIAN_POINT('Origin',(65.4714187197387,40.85,25.5142562776804)) ;
#11887 = CARTESIAN_POINT('Origin',(55.25,25.5,25.5)) ;
#11888 = CARTESIAN_POINT('',(76.5,10.,25.5)) ;
#11889 = CARTESIAN_POINT('Origin',(76.5,25.5,25.5)) ;
#11890 = CARTESIAN_POINT('',(45.75,10.,25.5)) ;
#11891 = CARTESIAN_POINT('',(55.25,10.,25.5)) ;
#11892 = CARTESIAN_POINT('Origin',(45.75,25.5,25.5)) ;
#11893 = CARTESIAN_POINT('',(48.2806275524199,40.9807202883652,24.7271485567093)) ;
#11894 = CARTESIAN_POINT('',(48.2806275524199,40.9609184856404,26.5999998092651)) ;
#11895 = CARTESIAN_POINT('Origin',(48.2806275524199,25.5,25.5)) ;
#11896 = CARTESIAN_POINT('',(48.,40.9609184856404,26.5999998092651)) ;
#11897 = CARTESIAN_POINT('',(55.25,40.9609184856404,26.5999998092651)) ;
#11898 = CARTESIAN_POINT('',(48.,40.960918459348,24.3999998211861)) ;
#11899 = CARTESIAN_POINT('Origin',(48.,25.5,25.5)) ;
#11900 = CARTESIAN_POINT('',(48.438199210912,40.960918459348,24.3999998211861)) ;
#11901 = CARTESIAN_POINT('',(55.25,40.960918459348,24.3999998211861)) ;
#11902 = CARTESIAN_POINT('',(48.9589358605444,40.99324057365,25.9577079057693)) ;
#11903 = CARTESIAN_POINT('Origin',(48.8059256247246,25.5,25.5)) ;
#11904 = CARTESIAN_POINT('',(49.0639836080372,40.9801923016591,26.2833557963371)) ;
#11905 = CARTESIAN_POINT('Ctrl Pts',(48.9589358605444,40.99324057365,25.9577079057693)) ;
#11906 = CARTESIAN_POINT('Ctrl Pts',(48.9648960688367,40.9927086680923,25.975712708973)) ;
#11907 = CARTESIAN_POINT('Ctrl Pts',(48.9708344768427,40.9921439425243,25.9936940683478)) ;
#11908 = CARTESIAN_POINT('Ctrl Pts',(48.9767569444717,40.991548248129,26.0116790190537)) ;
#11909 = CARTESIAN_POINT('Ctrl Pts',(48.9825218268715,40.9909684039913,26.0291854255518)) ;
#11910 = CARTESIAN_POINT('Ctrl Pts',(48.9882716861526,40.99035921714,26.046695460152)) ;
#11911 = CARTESIAN_POINT('Ctrl Pts',(48.9939957694241,40.9897223948859,26.0641886918098)) ;
#11912 = CARTESIAN_POINT('Ctrl Pts',(48.9994822498152,40.9891120066991,26.0809557910841)) ;
#11913 = CARTESIAN_POINT('Ctrl Pts',(49.0049450898077,40.9884762297473,26.0977075661051)) ;
#11914 = CARTESIAN_POINT('Ctrl Pts',(49.0103589727826,40.9878165674366,26.114381529626)) ;
#11915 = CARTESIAN_POINT('Ctrl Pts',(49.0139965926115,40.9873733364482,26.1255848638339)) ;
#11916 = CARTESIAN_POINT('Ctrl Pts',(49.0176117903286,40.986919322235,26.1367521707152)) ;
#11917 = CARTESIAN_POINT('Ctrl Pts',(49.0211924119893,40.9864549808355,26.1478519325859)) ;
#11918 = CARTESIAN_POINT('Ctrl Pts',(49.0253129741132,40.9859206189943,26.1606254849691)) ;
#11919 = CARTESIAN_POINT('Ctrl Pts',(49.0294779792121,40.9853585879042,26.1735890327011)) ;
#11920 = CARTESIAN_POINT('Ctrl Pts',(49.0336464350274,40.984777385263,26.1866349356787)) ;
#11921 = CARTESIAN_POINT('Ctrl Pts',(49.0377005191652,40.9842121293234,26.1993228927225)) ;
#11922 = CARTESIAN_POINT('Ctrl Pts',(49.0417579539094,40.9836287394359,26.2120889910656)) ;
#11923 = CARTESIAN_POINT('Ctrl Pts',(49.0457648803463,40.9830350328495,26.2247888680327)) ;
#11924 = CARTESIAN_POINT('Ctrl Pts',(49.0496161917,40.9824643837614,26.2369955259596)) ;
#11925 = CARTESIAN_POINT('Ctrl Pts',(49.0534208832824,40.9818842037434,26.249141122998)) ;
#11926 = CARTESIAN_POINT('Ctrl Pts',(49.0571151352053,40.9813014341738,26.2610525607634)) ;
#11927 = CARTESIAN_POINT('Ctrl Pts',(49.059455920885,40.9809321743909,26.2685999948659)) ;
#11928 = CARTESIAN_POINT('Ctrl Pts',(49.0617520462778,40.9805618749396,26.2760525179566)) ;
#11929 = CARTESIAN_POINT('Ctrl Pts',(49.0639836080372,40.9801923016591,26.2833557963371)) ;
#11930 = CARTESIAN_POINT('',(49.1810368485749,40.9940150133522,25.9306956768036)) ;
#11931 = CARTESIAN_POINT('Ctrl Pts',(49.0639836080372,40.9801923016591,26.2833557963371)) ;
#11932 = CARTESIAN_POINT('Ctrl Pts',(49.0681377308435,40.9808649857505,26.2700626297562)) ;
#11933 = CARTESIAN_POINT('Ctrl Pts',(49.0724784462548,40.9815364180603,26.2563729913517)) ;
#11934 = CARTESIAN_POINT('Ctrl Pts',(49.0769179212993,40.9821984510247,26.2425153748387)) ;
#11935 = CARTESIAN_POINT('Ctrl Pts',(49.0814599230219,40.9828757731934,26.2283377260306)) ;
#11936 = CARTESIAN_POINT('Ctrl Pts',(49.0861053808611,40.9835432568605,26.2139840305657)) ;
#11937 = CARTESIAN_POINT('Ctrl Pts',(49.0907797150059,40.984192176838,26.1996468023641)) ;
#11938 = CARTESIAN_POINT('Ctrl Pts',(49.0956286721937,40.9848653390664,26.1847739662365)) ;
#11939 = CARTESIAN_POINT('Ctrl Pts',(49.1005087548046,40.9855185246986,26.1699187132935)) ;
#11940 = CARTESIAN_POINT('Ctrl Pts',(49.1053564565797,40.9861419936983,26.1552430524173)) ;
#11941 = CARTESIAN_POINT('Ctrl Pts',(49.1075732656997,40.986427100297,26.1485320086314)) ;
#11942 = CARTESIAN_POINT('Ctrl Pts',(49.1097835645299,40.9867059927074,26.1418578210392)) ;
#11943 = CARTESIAN_POINT('Ctrl Pts',(49.1119825312423,40.9869777395263,26.1352326309442)) ;
#11944 = CARTESIAN_POINT('Ctrl Pts',(49.1180615069825,40.9877289752363,26.116917497007)) ;
#11945 = CARTESIAN_POINT('Ctrl Pts',(49.124231241269,40.9884516561393,26.0984420610299)) ;
#11946 = CARTESIAN_POINT('Ctrl Pts',(49.1304495084946,40.9891439670279,26.0799090634785)) ;
#11947 = CARTESIAN_POINT('Ctrl Pts',(49.1368305907441,40.98985440493,26.0608908100947)) ;
#11948 = CARTESIAN_POINT('Ctrl Pts',(49.1432628771849,40.9905328616201,26.0418116829618)) ;
#11949 = CARTESIAN_POINT('Ctrl Pts',(49.1497204499148,40.9911773755401,26.0227299055392)) ;
#11950 = CARTESIAN_POINT('Ctrl Pts',(49.1564364380756,40.9918476812474,26.0028845245242)) ;
#11951 = CARTESIAN_POINT('Ctrl Pts',(49.1631798324207,40.9924812732244,25.9830361278838)) ;
#11952 = CARTESIAN_POINT('Ctrl Pts',(49.1699413896424,40.9930759448742,25.9631968758645)) ;
#11953 = CARTESIAN_POINT('Ctrl Pts',(49.1736338692995,40.9934006944693,25.9523626801179)) ;
#11954 = CARTESIAN_POINT('Ctrl Pts',(49.1773321021792,40.993713837084,25.9415303098698)) ;
#11955 = CARTESIAN_POINT('Ctrl Pts',(49.1810368485749,40.9940150133522,25.9306956768036)) ;
#11956 = CARTESIAN_POINT('',(49.7077762074769,40.960918459348,24.3999998211861)) ;
#11957 = CARTESIAN_POINT('Origin',(49.3292468040986,25.5,25.5)) ;
#11958 = CARTESIAN_POINT('',(50.0994542725384,40.960918459348,24.3999998211861)) ;
#11959 = CARTESIAN_POINT('',(55.25,40.960918459348,24.3999998211861)) ;
#11960 = CARTESIAN_POINT('',(50.0994542725384,40.9609184856404,26.5999998092651)) ;
#11961 = CARTESIAN_POINT('Origin',(50.0994542725384,25.5,25.5)) ;
#11962 = CARTESIAN_POINT('',(49.8188268132508,40.9609184856404,26.5999998092651)) ;
#11963 = CARTESIAN_POINT('',(55.25,40.9609184856404,26.5999998092651)) ;
#11964 = CARTESIAN_POINT('',(49.8188268132508,40.9822614389786,24.7586628735065)) ;
#11965 = CARTESIAN_POINT('Origin',(49.8188268132508,25.5,25.5)) ;
#11966 = CARTESIAN_POINT('',(49.179536152631,40.9609184856404,26.5999998092651)) ;
#11967 = CARTESIAN_POINT('Origin',(49.5614432284574,25.5,25.5)) ;
#11968 = CARTESIAN_POINT('',(48.916916821152,40.9609184856404,26.5999998092651)) ;
#11969 = CARTESIAN_POINT('',(55.25,40.9609184856404,26.5999998092651)) ;
#11970 = CARTESIAN_POINT('Origin',(48.5431989013291,25.5,25.5)) ;
#11971 = CARTESIAN_POINT('',(51.7614599056542,40.9643621744601,26.5504772901535)) ;
#11972 = CARTESIAN_POINT('',(51.4448158927262,40.9799256191272,26.2886081576347)) ;
#11973 = CARTESIAN_POINT('Ctrl Pts',(51.7614599056542,40.9643621744601,26.5504772901535)) ;
#11974 = CARTESIAN_POINT('Ctrl Pts',(51.6964813536973,40.9662655725095,26.5224568492794)) ;
#11975 = CARTESIAN_POINT('Ctrl Pts',(51.6359558815656,40.9686336795545,26.4866160640346)) ;
#11976 = CARTESIAN_POINT('Ctrl Pts',(51.581440855625,40.9713767366872,26.4415422834339)) ;
#11977 = CARTESIAN_POINT('Ctrl Pts',(51.5281656401324,40.9740574097187,26.3974935953311)) ;
#11978 = CARTESIAN_POINT('Ctrl Pts',(51.4827528621409,40.9769824160316,26.3463815455476)) ;
#11979 = CARTESIAN_POINT('Ctrl Pts',(51.4448158927262,40.9799256191272,26.2886081576347)) ;
#11980 = CARTESIAN_POINT('',(51.3240109868348,40.9950124467317,25.8931784272194)) ;
#11981 = CARTESIAN_POINT('Ctrl Pts',(51.4448158927262,40.9799256191272,26.2886081576347)) ;
#11982 = CARTESIAN_POINT('Ctrl Pts',(51.4068025882613,40.9828747393755,26.2307186194111)) ;
#11983 = CARTESIAN_POINT('Ctrl Pts',(51.3775082128716,40.9857098719761,26.1687185433935)) ;
#11984 = CARTESIAN_POINT('Ctrl Pts',(51.3572563430792,40.9882866323644,26.1024758864232)) ;
#11985 = CARTESIAN_POINT('Ctrl Pts',(51.3364460712854,40.9909344414101,26.0344067298455)) ;
#11986 = CARTESIAN_POINT('Ctrl Pts',(51.3259478200354,40.9932063396208,25.9643564223097)) ;
#11987 = CARTESIAN_POINT('Ctrl Pts',(51.3240109868348,40.9950124467317,25.8931784272194)) ;
#11988 = CARTESIAN_POINT('',(51.5986358113587,40.9956030954071,25.8691675901413)) ;
#11989 = CARTESIAN_POINT('Origin',(55.8210035835746,25.5,25.5)) ;
#11990 = CARTESIAN_POINT('',(51.6894270963967,40.9867797701289,26.1400408983231)) ;
#11991 = CARTESIAN_POINT('Ctrl Pts',(51.5986358113587,40.9956030954071,25.8691675901413)) ;
#11992 = CARTESIAN_POINT('Ctrl Pts',(51.6046370539695,40.9943933193175,25.9199472647895)) ;
#11993 = CARTESIAN_POINT('Ctrl Pts',(51.6148318747084,40.9929206486228,25.9709173464044)) ;
#11994 = CARTESIAN_POINT('Ctrl Pts',(51.6310807803016,40.9912950366146,26.019401663994)) ;
#11995 = CARTESIAN_POINT('Ctrl Pts',(51.6453470747562,40.9898677737479,26.0619701648198)) ;
#11996 = CARTESIAN_POINT('Ctrl Pts',(51.6643402765475,40.9883185923293,26.1028067144042)) ;
#11997 = CARTESIAN_POINT('Ctrl Pts',(51.6894270963967,40.9867797701289,26.1400408983231)) ;
#11998 = CARTESIAN_POINT('',(51.9107775874436,40.9787624461282,26.3111184477806)) ;
#11999 = CARTESIAN_POINT('Ctrl Pts',(51.6894270963967,40.9867797701289,26.1400408983231)) ;
#12000 = CARTESIAN_POINT('Ctrl Pts',(51.7142620765023,40.9852564000361,26.1769011945908)) ;
#12001 = CARTESIAN_POINT('Ctrl Pts',(51.7452172284269,40.9838223504436,26.2085097613467)) ;
#12002 = CARTESIAN_POINT('Ctrl Pts',(51.7803864227145,40.9825306087772,26.235694194809)) ;
#12003 = CARTESIAN_POINT('Ctrl Pts',(51.8201118378289,40.9810715200789,26.2664004115936)) ;
#12004 = CARTESIAN_POINT('Ctrl Pts',(51.8647416209425,40.979811830078,26.2910928092094)) ;
#12005 = CARTESIAN_POINT('Ctrl Pts',(51.9107775874436,40.9787624461282,26.3111184477806)) ;
#12006 = CARTESIAN_POINT('',(52.248431045562,40.9752035998426,26.3763980507851)) ;
#12007 = CARTESIAN_POINT('Ctrl Pts',(51.9107775874436,40.9787624461282,26.3111184477806)) ;
#12008 = CARTESIAN_POINT('Ctrl Pts',(51.9620215954958,40.9775943478592,26.3334095393825)) ;
#12009 = CARTESIAN_POINT('Ctrl Pts',(52.0153352704738,40.9767090178051,26.3494650680102)) ;
#12010 = CARTESIAN_POINT('Ctrl Pts',(52.070210135829,40.9761193640483,26.3600752465508)) ;
#12011 = CARTESIAN_POINT('Ctrl Pts',(52.128909533513,40.9754886140657,26.3714249070122)) ;
#12012 = CARTESIAN_POINT('Ctrl Pts',(52.1886446082517,40.9752035998426,26.3763980507851)) ;
#12013 = CARTESIAN_POINT('Ctrl Pts',(52.248431045562,40.9752035998426,26.3763980507851)) ;
#12014 = CARTESIAN_POINT('',(52.5425647683442,40.9779286844934,26.3268758296967)) ;
#12015 = CARTESIAN_POINT('Ctrl Pts',(52.248431045562,40.9752035998426,26.3763980507851)) ;
#12016 = CARTESIAN_POINT('Ctrl Pts',(52.3008462457101,40.9752035998426,26.3763980507851)) ;
#12017 = CARTESIAN_POINT('Ctrl Pts',(52.3535603822056,40.9754138750608,26.3727206746845)) ;
#12018 = CARTESIAN_POINT('Ctrl Pts',(52.4052520979163,40.97589976934,26.3640175515236)) ;
#12019 = CARTESIAN_POINT('Ctrl Pts',(52.4521459373439,40.9763405643107,26.3561222272069)) ;
#12020 = CARTESIAN_POINT('Ctrl Pts',(52.4982385886269,40.9770093346525,26.3440847391397)) ;
#12021 = CARTESIAN_POINT('Ctrl Pts',(52.5425647683442,40.9779286844934,26.3268758296967)) ;
#12022 = CARTESIAN_POINT('',(52.7324010916054,40.9845868720206,26.1910639643669)) ;
#12023 = CARTESIAN_POINT('Ctrl Pts',(52.5425647683442,40.9779286844934,26.3268758296967)) ;
#12024 = CARTESIAN_POINT('Ctrl Pts',(52.5816398844146,40.9787391273113,26.3117055034049)) ;
#12025 = CARTESIAN_POINT('Ctrl Pts',(52.6197003909076,40.9797431606842,26.292557929649)) ;
#12026 = CARTESIAN_POINT('Ctrl Pts',(52.6537956587279,40.9809534520937,26.2681667879486)) ;
#12027 = CARTESIAN_POINT('Ctrl Pts',(52.6839651701171,40.9820243895815,26.2465840618294)) ;
#12028 = CARTESIAN_POINT('Ctrl Pts',(52.7106959059527,40.9832447154609,26.2211375044691)) ;
#12029 = CARTESIAN_POINT('Ctrl Pts',(52.7324010916054,40.9845868720206,26.1910639643669)) ;
#12030 = CARTESIAN_POINT('',(52.7946796007454,40.9918450924657,26.0027281880379)) ;
#12031 = CARTESIAN_POINT('Ctrl Pts',(52.7324010916054,40.9845868720206,26.1910639643669)) ;
#12032 = CARTESIAN_POINT('Ctrl Pts',(52.7524211406543,40.9858248209608,26.1633253918234)) ;
#12033 = CARTESIAN_POINT('Ctrl Pts',(52.7683641209573,40.987089895988,26.1333269333519)) ;
#12034 = CARTESIAN_POINT('Ctrl Pts',(52.7791056990498,40.9883498589597,26.100848272414)) ;
#12035 = CARTESIAN_POINT('Ctrl Pts',(52.7896347238596,40.989584889909,26.0690122959998)) ;
#12036 = CARTESIAN_POINT('Ctrl Pts',(52.7946796007454,40.9907567799209,26.036265136544)) ;
#12037 = CARTESIAN_POINT('Ctrl Pts',(52.7946796007454,40.9918450924657,26.0027281880379)) ;
#12038 = CARTESIAN_POINT('',(52.7346523590386,40.9966571536944,25.8218960404396)) ;
#12039 = CARTESIAN_POINT('Ctrl Pts',(52.7946796007454,40.9918450924657,26.0027281880379)) ;
#12040 = CARTESIAN_POINT('Ctrl Pts',(52.7946796007454,40.9929177965443,25.9696722229826)) ;
#12041 = CARTESIAN_POINT('Ctrl Pts',(52.7900915130482,40.993866440127,25.9371363688912)) ;
#12042 = CARTESIAN_POINT('Ctrl Pts',(52.7796755372991,40.9946882166121,25.9057549383327)) ;
#12043 = CARTESIAN_POINT('Ctrl Pts',(52.769538117278,40.9954880162271,25.8752127452538)) ;
#12044 = CARTESIAN_POINT('Ctrl Pts',(52.7543956539943,40.9961291401958,25.8473155645521)) ;
#12045 = CARTESIAN_POINT('Ctrl Pts',(52.7346523590386,40.9966571536944,25.8218960404396)) ;
#12046 = CARTESIAN_POINT('',(52.5365622825921,40.9988097137483,25.6920871078968)) ;
#12047 = CARTESIAN_POINT('Ctrl Pts',(52.7346523590386,40.9966571536944,25.8218960404396)) ;
#12048 = CARTESIAN_POINT('Ctrl Pts',(52.7129787665804,40.997236790954,25.7939912551781)) ;
#12049 = CARTESIAN_POINT('Ctrl Pts',(52.6854008743602,40.9976474971274,25.7707383845552)) ;
#12050 = CARTESIAN_POINT('Ctrl Pts',(52.6559042636246,40.9979624094066,25.7513188345919)) ;
#12051 = CARTESIAN_POINT('Ctrl Pts',(52.6233974190617,40.9983094596017,25.7299174506227)) ;
#12052 = CARTESIAN_POINT('Ctrl Pts',(52.5871671231961,40.9985539368512,25.7122615418921)) ;
#12053 = CARTESIAN_POINT('Ctrl Pts',(52.5507998661306,40.9987398284926,25.697652703815)) ;
#12054 = CARTESIAN_POINT('Ctrl Pts',(52.546053648936,40.9987640888349,25.6957461338928)) ;
#12055 = CARTESIAN_POINT('Ctrl Pts',(52.5413051382014,40.9987873513276,25.6938914502431)) ;
#12056 = CARTESIAN_POINT('Ctrl Pts',(52.5365622825921,40.9988097137483,25.6920871078968)) ;
#12057 = CARTESIAN_POINT('',(52.1448840685189,40.9997680931486,25.5847883164883)) ;
#12058 = CARTESIAN_POINT('Ctrl Pts',(52.5365622825921,40.9988097137483,25.6920871078968)) ;
#12059 = CARTESIAN_POINT('Ctrl Pts',(52.5182257411425,40.9988983054462,25.684938966189)) ;
#12060 = CARTESIAN_POINT('Ctrl Pts',(52.4945785983502,40.9989879874405,25.6771819864424)) ;
#12061 = CARTESIAN_POINT('Ctrl Pts',(52.4695770160932,40.9990711361368,25.6695822803517)) ;
#12062 = CARTESIAN_POINT('Ctrl Pts',(52.4546928281606,40.9991206370368,25.6650579485504)) ;
#12063 = CARTESIAN_POINT('Ctrl Pts',(52.4393314158557,40.9991678224209,25.6605898588925)) ;
#12064 = CARTESIAN_POINT('Ctrl Pts',(52.4243063105268,40.9992110837459,25.6563358768948)) ;
#12065 = CARTESIAN_POINT('Ctrl Pts',(52.4140931288561,40.9992404902467,25.653444270479)) ;
#12066 = CARTESIAN_POINT('Ctrl Pts',(52.4040348829017,40.9992680836439,25.6506515110719)) ;
#12067 = CARTESIAN_POINT('Ctrl Pts',(52.3943729570076,40.9992933587377,25.6480046613764)) ;
#12068 = CARTESIAN_POINT('Ctrl Pts',(52.3677500724645,40.9993630028139,25.6407114183296)) ;
#12069 = CARTESIAN_POINT('Ctrl Pts',(52.3394635166996,40.999428272284,25.6332473779268)) ;
#12070 = CARTESIAN_POINT('Ctrl Pts',(52.3106235865612,40.9994881370534,25.6258289117774)) ;
#12071 = CARTESIAN_POINT('Ctrl Pts',(52.268939054618,40.9995746641316,25.6151064416574)) ;
#12072 = CARTESIAN_POINT('Ctrl Pts',(52.2261050593121,40.9996499001918,25.6044803575766)) ;
#12073 = CARTESIAN_POINT('Ctrl Pts',(52.1855915980078,40.9997107348117,25.5946249394643)) ;
#12074 = CARTESIAN_POINT('Ctrl Pts',(52.1717040291299,40.9997315882502,25.5912466105472)) ;
#12075 = CARTESIAN_POINT('Ctrl Pts',(52.1580891323526,40.9997507494576,25.5879588380836)) ;
#12076 = CARTESIAN_POINT('Ctrl Pts',(52.1448840685189,40.9997680931486,25.5847883164883)) ;
#12077 = CARTESIAN_POINT('',(51.7201911397278,40.9999110068208,25.4474759042263)) ;
#12078 = CARTESIAN_POINT('Ctrl Pts',(52.1448840685189,40.9997680931486,25.5847883164883)) ;
#12079 = CARTESIAN_POINT('Ctrl Pts',(52.096230338235,40.9998319955481,25.5731066082814)) ;
#12080 = CARTESIAN_POINT('Ctrl Pts',(52.0446116326547,40.9998898156088,25.5600316125952)) ;
#12081 = CARTESIAN_POINT('Ctrl Pts',(51.9937884549582,40.9999317100544,25.5459097913523)) ;
#12082 = CARTESIAN_POINT('Ctrl Pts',(51.9573724589345,40.999961728405,25.5357911759974)) ;
#12083 = CARTESIAN_POINT('Ctrl Pts',(51.9213699605045,40.9999835704527,25.5251353447576)) ;
#12084 = CARTESIAN_POINT('Ctrl Pts',(51.8871420945215,40.9999936151787,25.5140687391253)) ;
#12085 = CARTESIAN_POINT('Ctrl Pts',(51.8629486620922,41.0000007151363,25.506246481795)) ;
#12086 = CARTESIAN_POINT('Ctrl Pts',(51.8383934367245,41.0000022794694,25.4978174129243)) ;
#12087 = CARTESIAN_POINT('Ctrl Pts',(51.8145911107741,40.9999958146662,25.4888742637738)) ;
#12088 = CARTESIAN_POINT('Ctrl Pts',(51.7804331295751,40.9999865372272,25.4760402272524)) ;
#12089 = CARTESIAN_POINT('Ctrl Pts',(51.7478284878484,40.999960724399,25.4621476092093)) ;
#12090 = CARTESIAN_POINT('Ctrl Pts',(51.7201911397278,40.9999110068208,25.4474759042263)) ;
#12091 = CARTESIAN_POINT('',(51.4853342361748,40.9978631490248,25.2426329195499)) ;
#12092 = CARTESIAN_POINT('Ctrl Pts',(51.7201911397278,40.9999110068208,25.4474759042263)) ;
#12093 = CARTESIAN_POINT('Ctrl Pts',(51.6712001615781,40.9998240471528,25.4218140228572)) ;
#12094 = CARTESIAN_POINT('Ctrl Pts',(51.6243780826768,40.9996618864735,25.3913559963214)) ;
#12095 = CARTESIAN_POINT('Ctrl Pts',(51.5826913086288,40.9993217284307,25.3549966945329)) ;
#12096 = CARTESIAN_POINT('Ctrl Pts',(51.5450120776924,40.9990142713597,25.3221327812161)) ;
#12097 = CARTESIAN_POINT('Ctrl Pts',(51.5120411777685,40.9985650171349,25.2848972833514)) ;
#12098 = CARTESIAN_POINT('Ctrl Pts',(51.4853342361748,40.9978631490248,25.2426329195499)) ;
#12099 = CARTESIAN_POINT('',(51.4080490656197,40.990893529069,24.9687583684921)) ;
#12100 = CARTESIAN_POINT('Ctrl Pts',(51.4853342361748,40.9978631490248,25.2426329195499)) ;
#12101 = CARTESIAN_POINT('Ctrl Pts',(51.4597867312913,40.9971917513319,25.2022033916376)) ;
#12102 = CARTESIAN_POINT('Ctrl Pts',(51.4403592614856,40.9963177393255,25.1590373372296)) ;
#12103 = CARTESIAN_POINT('Ctrl Pts',(51.4273724576651,40.9951684612961,25.1130189202868)) ;
#12104 = CARTESIAN_POINT('Ctrl Pts',(51.4140845004671,40.9939925324474,25.065933373827)) ;
#12105 = CARTESIAN_POINT('Ctrl Pts',(51.4080490656197,40.9925708016359,25.0176672815208)) ;
#12106 = CARTESIAN_POINT('Ctrl Pts',(51.4080490656197,40.990893529069,24.9687583684921)) ;
#12107 = CARTESIAN_POINT('',(51.5025921650231,40.9770788394087,24.6573668658733)) ;
#12108 = CARTESIAN_POINT('Ctrl Pts',(51.4080490656197,40.990893529069,24.9687583684921)) ;
#12109 = CARTESIAN_POINT('Ctrl Pts',(51.4080490656197,40.9890120993808,24.913896277019)) ;
#12110 = CARTESIAN_POINT('Ctrl Pts',(51.4157405734043,40.9868770379277,24.8601568119043)) ;
#12111 = CARTESIAN_POINT('Ctrl Pts',(51.4316684952429,40.9845306068251,24.8076764583681)) ;
#12112 = CARTESIAN_POINT('Ctrl Pts',(51.447903294973,40.9821389678267,24.7541849835815)) ;
#12113 = CARTESIAN_POINT('Ctrl Pts',(51.4720374059445,40.9796269269382,24.704168908171)) ;
#12114 = CARTESIAN_POINT('Ctrl Pts',(51.5025921650231,40.9770788394087,24.6573668658733)) ;
#12115 = CARTESIAN_POINT('',(51.7787178345025,40.9635419522324,24.4375169217587)) ;
#12116 = CARTESIAN_POINT('Ctrl Pts',(51.5025921650231,40.9770788394087,24.6573668658733)) ;
#12117 = CARTESIAN_POINT('Ctrl Pts',(51.5344017011208,40.9744261081125,24.6086427773617)) ;
#12118 = CARTESIAN_POINT('Ctrl Pts',(51.5732894347549,40.9718958869814,24.5663202911221)) ;
#12119 = CARTESIAN_POINT('Ctrl Pts',(51.6188180475123,40.9696222373288,24.5300578190727)) ;
#12120 = CARTESIAN_POINT('Ctrl Pts',(51.6672834699504,40.9672019265788,24.4914562470045)) ;
#12121 = CARTESIAN_POINT('Ctrl Pts',(51.7214359964055,40.9651683030504,24.4611870814236)) ;
#12122 = CARTESIAN_POINT('Ctrl Pts',(51.7787178345025,40.9635419522324,24.4375169217587)) ;
#12123 = CARTESIAN_POINT('',(52.1824010200799,40.958203478351,24.3624828696251)) ;
#12124 = CARTESIAN_POINT('Ctrl Pts',(51.7787178345025,40.9635419522324,24.4375169217587)) ;
#12125 = CARTESIAN_POINT('Ctrl Pts',(51.8405473847017,40.9617864795045,24.4119675019799)) ;
#12126 = CARTESIAN_POINT('Ctrl Pts',(51.90459885672,40.9604580977664,24.3934803221617)) ;
#12127 = CARTESIAN_POINT('Ctrl Pts',(51.9703891248391,40.9595729585521,24.3812489377864)) ;
#12128 = CARTESIAN_POINT('Ctrl Pts',(52.040299600929,40.9586323862509,24.3682515457805)) ;
#12129 = CARTESIAN_POINT('Ctrl Pts',(52.1112893721457,40.958203478351,24.3624828696251)) ;
#12130 = CARTESIAN_POINT('Ctrl Pts',(52.1824010200799,40.958203478351,24.3624828696251)) ;
#12131 = CARTESIAN_POINT('',(52.6138474531472,40.9637992678179,24.4412685871124)) ;
#12132 = CARTESIAN_POINT('Ctrl Pts',(52.1824010200799,40.958203478351,24.3624828696251)) ;
#12133 = CARTESIAN_POINT('Ctrl Pts',(52.25942789036,40.958203478351,24.3624828696251)) ;
#12134 = CARTESIAN_POINT('Ctrl Pts',(52.3367901435739,40.9586397198479,24.3683417117733)) ;
#12135 = CARTESIAN_POINT('Ctrl Pts',(52.4125663074585,40.959640229793,24.3821789206829)) ;
#12136 = CARTESIAN_POINT('Ctrl Pts',(52.481642392275,40.9605522753003,24.3947926525909)) ;
#12137 = CARTESIAN_POINT('Ctrl Pts',(52.5491617482125,40.9619317389306,24.4139915161869)) ;
#12138 = CARTESIAN_POINT('Ctrl Pts',(52.6138474531472,40.9637992678179,24.4412685871124)) ;
#12139 = CARTESIAN_POINT('',(52.901227671653,40.9779286727117,24.6731239497662)) ;
#12140 = CARTESIAN_POINT('Ctrl Pts',(52.6138474531472,40.9637992678179,24.4412685871124)) ;
#12141 = CARTESIAN_POINT('Ctrl Pts',(52.6731688875777,40.9655119290941,24.4662836663549)) ;
#12142 = CARTESIAN_POINT('Ctrl Pts',(52.728970455649,40.9676436064132,24.4981815551952)) ;
#12143 = CARTESIAN_POINT('Ctrl Pts',(52.7790628186729,40.9701546747433,24.5385873209086)) ;
#12144 = CARTESIAN_POINT('Ctrl Pts',(52.8267918049618,40.9725472699148,24.5770867272315)) ;
#12145 = CARTESIAN_POINT('Ctrl Pts',(52.8675699374113,40.9751912656509,24.6218836324023)) ;
#12146 = CARTESIAN_POINT('Ctrl Pts',(52.901227671653,40.9779286727117,24.6731239497662)) ;
#12147 = CARTESIAN_POINT('',(53.0092771835625,40.9925591905437,25.0197815835476)) ;
#12148 = CARTESIAN_POINT('Ctrl Pts',(52.901227671653,40.9779286727117,24.6731239497662)) ;
#12149 = CARTESIAN_POINT('Ctrl Pts',(52.9345738501646,40.9806407272898,24.7238897051711)) ;
#12150 = CARTESIAN_POINT('Ctrl Pts',(52.9603936002435,40.9832945476178,24.778224903136)) ;
#12151 = CARTESIAN_POINT('Ctrl Pts',(52.9784800908764,40.9857803484854,24.8362176573139)) ;
#12152 = CARTESIAN_POINT('Ctrl Pts',(52.9970861473933,40.9883375583042,24.8958763541669)) ;
#12153 = CARTESIAN_POINT('Ctrl Pts',(53.0068559081193,40.9906229160949,24.957314494657)) ;
#12154 = CARTESIAN_POINT('Ctrl Pts',(53.0092771835625,40.9925591905437,25.0197815835475)) ;
#12155 = CARTESIAN_POINT('',(52.7301501221955,40.993196160172,25.0407911777496)) ;
#12156 = CARTESIAN_POINT('Origin',(46.6292417526227,25.5,25.5)) ;
#12157 = CARTESIAN_POINT('',(52.5778307504952,40.9806452954799,24.7256478607655)) ;
#12158 = CARTESIAN_POINT('Ctrl Pts',(52.7301501221955,40.993196160172,25.0407911777496)) ;
#12159 = CARTESIAN_POINT('Ctrl Pts',(52.7233426866318,40.9913264464056,24.9777091097621)) ;
#12160 = CARTESIAN_POINT('Ctrl Pts',(52.7084515806111,40.9890587023187,24.9149092071746)) ;
#12161 = CARTESIAN_POINT('Ctrl Pts',(52.680844208208,40.986689065273,24.8577681138769)) ;
#12162 = CARTESIAN_POINT('Ctrl Pts',(52.6684313800218,40.9856236289438,24.8320763325977)) ;
#12163 = CARTESIAN_POINT('Ctrl Pts',(52.6535949220013,40.9845538245761,24.8078292757448)) ;
#12164 = CARTESIAN_POINT('Ctrl Pts',(52.6360497020993,40.9835151584649,24.7853264118589)) ;
#12165 = CARTESIAN_POINT('Ctrl Pts',(52.6188579928331,40.9824974199636,24.7632769479167)) ;
#12166 = CARTESIAN_POINT('Ctrl Pts',(52.5994458221421,40.9815327548068,24.7433897153539)) ;
#12167 = CARTESIAN_POINT('Ctrl Pts',(52.5778307504952,40.9806452954799,24.7256478607655)) ;
#12168 = CARTESIAN_POINT('',(52.1944065876305,40.9749479577385,24.6190994918346)) ;
#12169 = CARTESIAN_POINT('Ctrl Pts',(52.5778307504952,40.9806452954799,24.7256478607655)) ;
#12170 = CARTESIAN_POINT('Ctrl Pts',(52.5404445771057,40.9791103138436,24.6949609096451)) ;
#12171 = CARTESIAN_POINT('Ctrl Pts',(52.4974914881731,40.977912081391,24.6726577834149)) ;
#12172 = CARTESIAN_POINT('Ctrl Pts',(52.451846940174,40.9770388904196,24.656633422266)) ;
#12173 = CARTESIAN_POINT('Ctrl Pts',(52.4149548595667,40.9763331362143,24.6436817763608)) ;
#12174 = CARTESIAN_POINT('Ctrl Pts',(52.3760168414359,40.9758364044645,24.6347357031708)) ;
#12175 = CARTESIAN_POINT('Ctrl Pts',(52.3364479207098,40.9755047478818,24.6288393623379)) ;
#12176 = CARTESIAN_POINT('Ctrl Pts',(52.2891833143096,40.9751085880283,24.6217962531615)) ;
#12177 = CARTESIAN_POINT('Ctrl Pts',(52.2410243634678,40.9749479577385,24.6190994918346)) ;
#12178 = CARTESIAN_POINT('Ctrl Pts',(52.1944065876305,40.9749479577385,24.6190994918346)) ;
#12179 = CARTESIAN_POINT('',(51.8094815798104,40.9801542905129,24.7158934116364)) ;
#12180 = CARTESIAN_POINT('Ctrl Pts',(52.1944065876305,40.9749479577385,24.6190994918346)) ;
#12181 = CARTESIAN_POINT('Ctrl Pts',(52.1439402727095,40.9749479577385,24.6190994918346)) ;
#12182 = CARTESIAN_POINT('Ctrl Pts',(52.0910857438607,40.9751032396394,24.6217463705642)) ;
#12183 = CARTESIAN_POINT('Ctrl Pts',(52.0397048022768,40.975513640306,24.6290595674904)) ;
#12184 = CARTESIAN_POINT('Ctrl Pts',(52.0146784903811,40.9757135357296,24.632621634311)) ;
#12185 = CARTESIAN_POINT('Ctrl Pts',(51.9900025942792,40.9759739557623,24.6372912969542)) ;
#12186 = CARTESIAN_POINT('Ctrl Pts',(51.9661169206961,40.9763064369372,24.6432975603998)) ;
#12187 = CARTESIAN_POINT('Ctrl Pts',(51.9363088470246,40.9767213560861,24.6507930636208)) ;
#12188 = CARTESIAN_POINT('Ctrl Pts',(51.9067290064541,40.9772610647307,24.6606207748326)) ;
#12189 = CARTESIAN_POINT('Ctrl Pts',(51.8788404119519,40.9779512382307,24.6735464520297)) ;
#12190 = CARTESIAN_POINT('Ctrl Pts',(51.8541742294851,40.9785616650302,24.6849786205538)) ;
#12191 = CARTESIAN_POINT('Ctrl Pts',(51.830695022219,40.9792933473658,24.6988963184466)) ;
#12192 = CARTESIAN_POINT('Ctrl Pts',(51.8094815798104,40.9801542905129,24.7158934116364)) ;
#12193 = CARTESIAN_POINT('',(51.688676673919,40.9902121952529,24.9492494702339)) ;
#12194 = CARTESIAN_POINT('Ctrl Pts',(51.8094815798104,40.9801542905129,24.7158934116364)) ;
#12195 = CARTESIAN_POINT('Ctrl Pts',(51.7743817719654,40.9815788111055,24.7440168822091)) ;
#12196 = CARTESIAN_POINT('Ctrl Pts',(51.743699410759,40.9831904309469,24.7772470381369)) ;
#12197 = CARTESIAN_POINT('Ctrl Pts',(51.7220520990965,40.9849304145919,24.8166771954285)) ;
#12198 = CARTESIAN_POINT('Ctrl Pts',(51.7110076789359,40.9858181511731,24.8367943920077)) ;
#12199 = CARTESIAN_POINT('Ctrl Pts',(51.7026233497426,40.9867130969639,24.8579614264901)) ;
#12200 = CARTESIAN_POINT('Ctrl Pts',(51.6970205795988,40.9876036979261,24.8802164119748)) ;
#12201 = CARTESIAN_POINT('Ctrl Pts',(51.6913231790868,40.9885093410718,24.9028472824976)) ;
#12202 = CARTESIAN_POINT('Ctrl Pts',(51.688676673919,40.9893823612855,24.9259098572)) ;
#12203 = CARTESIAN_POINT('Ctrl Pts',(51.688676673919,40.9902121952529,24.9492494702339)) ;
#12204 = CARTESIAN_POINT('',(51.7742155976593,40.9959189676464,25.1443381547928)) ;
#12205 = CARTESIAN_POINT('Ctrl Pts',(51.688676673919,40.9902121952529,24.9492494702339)) ;
#12206 = CARTESIAN_POINT('Ctrl Pts',(51.688676673919,40.9914864166818,24.9850877658867)) ;
#12207 = CARTESIAN_POINT('Ctrl Pts',(51.6945391874085,40.9926057767986,25.0201432961235)) ;
#12208 = CARTESIAN_POINT('Ctrl Pts',(51.7083258839055,40.9935600903843,25.0532386256064)) ;
#12209 = CARTESIAN_POINT('Ctrl Pts',(51.7154858640819,40.9940557034093,25.0704263473408)) ;
#12210 = CARTESIAN_POINT('Ctrl Pts',(51.7245587420721,40.9944920818065,25.0865475195267)) ;
#12211 = CARTESIAN_POINT('Ctrl Pts',(51.7354721183132,40.9948800090314,25.1016364653763)) ;
#12212 = CARTESIAN_POINT('Ctrl Pts',(51.7467870555517,40.9952822101566,25.1172806135766)) ;
#12213 = CARTESIAN_POINT('Ctrl Pts',(51.759825949631,40.9956234625419,25.1314632197502)) ;
#12214 = CARTESIAN_POINT('Ctrl Pts',(51.7742155976593,40.9959189676464,25.1443381547928)) ;
#12215 = CARTESIAN_POINT('',(52.213165063411,40.9987245424185,25.301159465313)) ;
#12216 = CARTESIAN_POINT('Ctrl Pts',(51.7742155976593,40.9959189676464,25.1443381547928)) ;
#12217 = CARTESIAN_POINT('Ctrl Pts',(51.7845766428338,40.9961355419343,25.1537741335494)) ;
#12218 = CARTESIAN_POINT('Ctrl Pts',(51.7972705332651,40.9963287165035,25.1625669264881)) ;
#12219 = CARTESIAN_POINT('Ctrl Pts',(51.81087410563,40.9964999073154,25.1706209396928)) ;
#12220 = CARTESIAN_POINT('Ctrl Pts',(51.8177681697437,40.9965866639703,25.1747025795677)) ;
#12221 = CARTESIAN_POINT('Ctrl Pts',(51.8248962317976,40.9966677745506,25.1785944841596)) ;
#12222 = CARTESIAN_POINT('Ctrl Pts',(51.8320789274207,40.9967434233534,25.1822842925641)) ;
#12223 = CARTESIAN_POINT('Ctrl Pts',(51.8666642598451,40.9971076792165,25.2000510554829)) ;
#12224 = CARTESIAN_POINT('Ctrl Pts',(51.9106531996414,40.9974307096486,25.2173079842982)) ;
#12225 = CARTESIAN_POINT('Ctrl Pts',(51.961637056368,40.9977170699623,25.2339935089345)) ;
#12226 = CARTESIAN_POINT('Ctrl Pts',(52.0071481792142,40.9979726916482,25.2488879678913)) ;
#12227 = CARTESIAN_POINT('Ctrl Pts',(52.0582327363947,40.9981990932109,25.2633271053793)) ;
#12228 = CARTESIAN_POINT('Ctrl Pts',(52.1132190775607,40.9983995148573,25.2772677033774)) ;
#12229 = CARTESIAN_POINT('Ctrl Pts',(52.1453123943052,40.9985164929149,25.2854042699805)) ;
#12230 = CARTESIAN_POINT('Ctrl Pts',(52.17873570998,40.9986246206864,25.2933710161247)) ;
#12231 = CARTESIAN_POINT('Ctrl Pts',(52.213165063411,40.9987245424185,25.301159465313)) ;
#12232 = CARTESIAN_POINT('',(52.7001365013421,40.9998895035356,25.4414732694626)) ;
#12233 = CARTESIAN_POINT('Ctrl Pts',(52.213165063411,40.9987245424185,25.301159465313)) ;
#12234 = CARTESIAN_POINT('Ctrl Pts',(52.2588316805259,40.9988570774647,25.3114899755225)) ;
#12235 = CARTESIAN_POINT('Ctrl Pts',(52.307250337576,40.9989911466368,25.3228165607694)) ;
#12236 = CARTESIAN_POINT('Ctrl Pts',(52.3556913472795,40.9991187993419,25.3347995517285)) ;
#12237 = CARTESIAN_POINT('Ctrl Pts',(52.3948926984319,40.9992221035164,25.3444969019555)) ;
#12238 = CARTESIAN_POINT('Ctrl Pts',(52.4341033743883,40.9993212055398,25.354623649893)) ;
#12239 = CARTESIAN_POINT('Ctrl Pts',(52.4718855245653,40.9994118917176,25.3650005797862)) ;
#12240 = CARTESIAN_POINT('Ctrl Pts',(52.4855872668106,40.9994447791692,25.3687637859041)) ;
#12241 = CARTESIAN_POINT('Ctrl Pts',(52.4991015449596,40.9994765598033,25.3725599321762)) ;
#12242 = CARTESIAN_POINT('Ctrl Pts',(52.5123617001045,40.9995070326502,25.3763806454261)) ;
#12243 = CARTESIAN_POINT('Ctrl Pts',(52.5357625667123,40.9995608096249,25.3831232513858)) ;
#12244 = CARTESIAN_POINT('Ctrl Pts',(52.5597894438442,40.9996136590807,25.3903496797628)) ;
#12245 = CARTESIAN_POINT('Ctrl Pts',(52.583398610579,40.9996634459259,25.3979347181335)) ;
#12246 = CARTESIAN_POINT('Ctrl Pts',(52.6148861793824,40.99972984669,25.4080508912394)) ;
#12247 = CARTESIAN_POINT('Ctrl Pts',(52.645628605886,40.9997907998102,25.4188047506243)) ;
#12248 = CARTESIAN_POINT('Ctrl Pts',(52.6730448795419,40.9998412401404,25.4298897091704)) ;
#12249 = CARTESIAN_POINT('Ctrl Pts',(52.6825076792224,40.9998586497543,25.4337157120585)) ;
#12250 = CARTESIAN_POINT('Ctrl Pts',(52.6915737547063,40.9998748069759,25.4375811154143)) ;
#12251 = CARTESIAN_POINT('Ctrl Pts',(52.7001365013421,40.9998895035356,25.4414732694626)) ;
#12252 = CARTESIAN_POINT('',(52.9837652035058,40.9991129429665,25.6658251523972)) ;
#12253 = CARTESIAN_POINT('Ctrl Pts',(52.7001365013421,40.9998895035356,25.4414732694626)) ;
#12254 = CARTESIAN_POINT('Ctrl Pts',(52.759051244481,40.999992043072,25.4686292624549)) ;
#12255 = CARTESIAN_POINT('Ctrl Pts',(52.8161909873028,41.0000522044823,25.5015720568016)) ;
#12256 = CARTESIAN_POINT('Ctrl Pts',(52.8670872082483,40.9999435530579,25.5418312325623)) ;
#12257 = CARTESIAN_POINT('Ctrl Pts',(52.9119925723242,40.9998476906997,25.5773516093475)) ;
#12258 = CARTESIAN_POINT('Ctrl Pts',(52.9517624575517,40.9996209274521,25.6183455704352)) ;
#12259 = CARTESIAN_POINT('Ctrl Pts',(52.9837652035057,40.9991129429665,25.6658251523971)) ;
#12260 = CARTESIAN_POINT('',(53.0753072090447,40.9926056458522,25.9787173509598)) ;
#12261 = CARTESIAN_POINT('Ctrl Pts',(52.9837652035058,40.9991129429665,25.6658251523972)) ;
#12262 = CARTESIAN_POINT('Ctrl Pts',(53.0142076130435,40.9986297290861,25.7109895101566)) ;
#12263 = CARTESIAN_POINT('Ctrl Pts',(53.0371279248959,40.9979127094772,25.7596817012363)) ;
#12264 = CARTESIAN_POINT('Ctrl Pts',(53.052420112575,40.9968605874156,25.8119486082757)) ;
#12265 = CARTESIAN_POINT('Ctrl Pts',(53.0683053848871,40.995767660373,25.8662426091512)) ;
#12266 = CARTESIAN_POINT('Ctrl Pts',(53.0753072090447,40.9943530563869,25.9221663563878)) ;
#12267 = CARTESIAN_POINT('Ctrl Pts',(53.0753072090447,40.9926056458522,25.9787173509598)) ;
#12268 = CARTESIAN_POINT('',(52.974761325866,40.9788410048888,26.3096179008484)) ;
#12269 = CARTESIAN_POINT('Ctrl Pts',(53.0753072090447,40.9926056458522,25.9787173509598)) ;
#12270 = CARTESIAN_POINT('Ctrl Pts',(53.0753072090447,40.9908113092192,26.0367870026948)) ;
#12271 = CARTESIAN_POINT('Ctrl Pts',(53.0670587148995,40.9887277985932,26.0936344221622)) ;
#12272 = CARTESIAN_POINT('Ctrl Pts',(53.0501868887134,40.9863993988086,26.1491792206938)) ;
#12273 = CARTESIAN_POINT('Ctrl Pts',(53.0328659874607,40.9840090243286,26.2062024474536)) ;
#12274 = CARTESIAN_POINT('Ctrl Pts',(53.007140893577,40.9814572470054,26.2595987551357)) ;
#12275 = CARTESIAN_POINT('Ctrl Pts',(52.974761325866,40.9788410048888,26.3096179008484)) ;
#12276 = CARTESIAN_POINT('',(52.6858799643815,40.9643111807864,26.5512277126312)) ;
#12277 = CARTESIAN_POINT('Ctrl Pts',(52.974761325866,40.9788410048888,26.3096179008484)) ;
#12278 = CARTESIAN_POINT('Ctrl Pts',(52.9409768447557,40.9761112521767,26.361807221475)) ;
#12279 = CARTESIAN_POINT('Ctrl Pts',(52.9000470821262,40.9734504375446,26.4077057301649)) ;
#12280 = CARTESIAN_POINT('Ctrl Pts',(52.8523552454749,40.9710064235648,26.4476076413884)) ;
#12281 = CARTESIAN_POINT('Ctrl Pts',(52.8019258671075,40.9684221216301,26.4897999476604)) ;
#12282 = CARTESIAN_POINT('Ctrl Pts',(52.7456750630569,40.9661735116778,26.5238314938297)) ;
#12283 = CARTESIAN_POINT('Ctrl Pts',(52.6858799643815,40.9643111807864,26.5512277126312)) ;
#12284 = CARTESIAN_POINT('',(52.2619374580681,40.9582035055449,26.6375167608261)) ;
#12285 = CARTESIAN_POINT('Ctrl Pts',(52.6858799643815,40.9643111807864,26.5512277126312)) ;
#12286 = CARTESIAN_POINT('Ctrl Pts',(52.6217774636278,40.9623147018492,26.5805973450908)) ;
#12287 = CARTESIAN_POINT('Ctrl Pts',(52.5548956312819,40.9607923362899,26.6018617749191)) ;
#12288 = CARTESIAN_POINT('Ctrl Pts',(52.485782063455,40.9597766179076,26.6159332078567)) ;
#12289 = CARTESIAN_POINT('Ctrl Pts',(52.412126253308,40.9586941450635,26.6309294354505)) ;
#12290 = CARTESIAN_POINT('Ctrl Pts',(52.3371081527218,40.9582035055449,26.6375167608261)) ;
#12291 = CARTESIAN_POINT('Ctrl Pts',(52.2619374580681,40.9582035055449,26.6375167608261)) ;
#12292 = CARTESIAN_POINT('Ctrl Pts',(52.2619374580681,40.9582035055449,26.6375167608261)) ;
#12293 = CARTESIAN_POINT('Ctrl Pts',(52.1706029250554,40.9582035055449,26.6375167608261)) ;
#12294 = CARTESIAN_POINT('Ctrl Pts',(52.0775135059191,40.958659550423,26.631411163429)) ;
#12295 = CARTESIAN_POINT('Ctrl Pts',(51.9875030125669,40.959789307142,26.6157574013999)) ;
#12296 = CARTESIAN_POINT('Ctrl Pts',(51.9102085211818,40.9607594603733,26.6023150845183)) ;
#12297 = CARTESIAN_POINT('Ctrl Pts',(51.8334991343029,40.9622519469216,26.5815425242443)) ;
#12298 = CARTESIAN_POINT('Ctrl Pts',(51.7614599056542,40.9643621744601,26.5504772901535)) ;
#12299 = CARTESIAN_POINT('',(54.7800817079842,40.9828316466601,26.2293313384056)) ;
#12300 = CARTESIAN_POINT('',(54.9166436977684,40.9990723481228,25.6695769667625)) ;
#12301 = CARTESIAN_POINT('Ctrl Pts',(54.7800817079842,40.9828316466601,26.2293313384056)) ;
#12302 = CARTESIAN_POINT('Ctrl Pts',(54.8073320969825,40.9841999355338,26.2002842028176)) ;
#12303 = CARTESIAN_POINT('Ctrl Pts',(54.8283420621742,40.9857487026283,26.1655109637859)) ;
#12304 = CARTESIAN_POINT('Ctrl Pts',(54.8447345970925,40.9872223620408,26.1292404220201)) ;
#12305 = CARTESIAN_POINT('Ctrl Pts',(54.8590713359577,40.9885112090848,26.0975185871489)) ;
#12306 = CARTESIAN_POINT('Ctrl Pts',(54.8704235300848,40.9897852011198,26.0634298467531)) ;
#12307 = CARTESIAN_POINT('Ctrl Pts',(54.879448285824,40.9909699924001,26.0287344920374)) ;
#12308 = CARTESIAN_POINT('Ctrl Pts',(54.887578869659,40.9920373946778,25.9974767496277)) ;
#12309 = CARTESIAN_POINT('Ctrl Pts',(54.8938224906964,40.9930323965364,25.9657308124313)) ;
#12310 = CARTESIAN_POINT('Ctrl Pts',(54.898663241216,40.9939006335321,25.9347909362348)) ;
#12311 = CARTESIAN_POINT('Ctrl Pts',(54.9097428391148,40.9958878701713,25.8639751844412)) ;
#12312 = CARTESIAN_POINT('Ctrl Pts',(54.9147621112728,40.9974615661979,25.7890726554941)) ;
#12313 = CARTESIAN_POINT('Ctrl Pts',(54.9161937701846,40.998487528179,25.7162401478558)) ;
#12314 = CARTESIAN_POINT('Ctrl Pts',(54.9165017990757,40.9987082692569,25.7005698534987)) ;
#12315 = CARTESIAN_POINT('Ctrl Pts',(54.9166436977684,40.9989036547566,25.6849952793808)) ;
#12316 = CARTESIAN_POINT('Ctrl Pts',(54.9166436977684,40.9990723481228,25.6695769667625)) ;
#12317 = CARTESIAN_POINT('',(54.9166436977684,40.960918459348,24.3999998211861)) ;
#12318 = CARTESIAN_POINT('Origin',(54.9166436977684,25.5,25.5)) ;
#12319 = CARTESIAN_POINT('',(55.2077760286629,40.960918459348,24.3999998211861)) ;
#12320 = CARTESIAN_POINT('',(55.25,40.960918459348,24.3999998211861)) ;
#12321 = CARTESIAN_POINT('',(55.2077760286629,40.9990558578356,25.6710775136948)) ;
#12322 = CARTESIAN_POINT('Origin',(55.2077760286629,25.5,25.5)) ;
#12323 = CARTESIAN_POINT('',(55.132742125541,40.9842840200094,26.1978168725967)) ;
#12324 = CARTESIAN_POINT('Ctrl Pts',(55.2077760286629,40.9990558578356,25.6710775136948)) ;
#12325 = CARTESIAN_POINT('Ctrl Pts',(55.2077760286629,40.9983582600139,25.7342775647813)) ;
#12326 = CARTESIAN_POINT('Ctrl Pts',(55.2057352440292,40.9972316311301,25.7991446431383)) ;
#12327 = CARTESIAN_POINT('Ctrl Pts',(55.2005903188716,40.9957334148724,25.8632654607297)) ;
#12328 = CARTESIAN_POINT('Ctrl Pts',(55.197745628471,40.9949050332584,25.8987186245171)) ;
#12329 = CARTESIAN_POINT('Ctrl Pts',(55.1939513161689,40.9939630530806,25.9339424643913)) ;
#12330 = CARTESIAN_POINT('Ctrl Pts',(55.1890262614623,40.9929171841363,25.9685265472663)) ;
#12331 = CARTESIAN_POINT('Ctrl Pts',(55.1795591851992,40.9909067859485,26.0350050271158)) ;
#12332 = CARTESIAN_POINT('Ctrl Pts',(55.165290479564,40.9883698379393,26.1035339046001)) ;
#12333 = CARTESIAN_POINT('Ctrl Pts',(55.1435864745192,40.985607725278,26.1677518901363)) ;
#12334 = CARTESIAN_POINT('Ctrl Pts',(55.140160340722,40.9851717058649,26.177889162505)) ;
#12335 = CARTESIAN_POINT('Ctrl Pts',(55.1365489609818,40.9847300755964,26.1879190732343)) ;
#12336 = CARTESIAN_POINT('Ctrl Pts',(55.132742125541,40.9842840200094,26.1978168725967)) ;
#12337 = CARTESIAN_POINT('',(54.8618688173592,40.966717363426,26.5152113080025)) ;
#12338 = CARTESIAN_POINT('Ctrl Pts',(55.132742125541,40.9842840200094,26.1978168725967)) ;
#12339 = CARTESIAN_POINT('Ctrl Pts',(55.1077726684432,40.9813583150401,26.2627371238591)) ;
#12340 = CARTESIAN_POINT('Ctrl Pts',(55.0727465253504,40.9782964863988,26.321673362836)) ;
#12341 = CARTESIAN_POINT('Ctrl Pts',(55.0276078044709,40.9753058232692,26.3745911480752)) ;
#12342 = CARTESIAN_POINT('Ctrl Pts',(54.9801914455488,40.9721642553734,26.430179092292)) ;
#12343 = CARTESIAN_POINT('Ctrl Pts',(54.9238555967464,40.9692583682441,26.476499166963)) ;
#12344 = CARTESIAN_POINT('Ctrl Pts',(54.8618688173592,40.966717363426,26.5152113080025)) ;
#12345 = CARTESIAN_POINT('',(54.3478848524392,40.9582035055449,26.6375167608261)) ;
#12346 = CARTESIAN_POINT('Ctrl Pts',(54.8618688173592,40.966717363426,26.5152113080025)) ;
#12347 = CARTESIAN_POINT('Ctrl Pts',(54.7923268047314,40.9638666562218,26.558641756684)) ;
#12348 = CARTESIAN_POINT('Ctrl Pts',(54.7153634299227,40.9617853612427,26.5879136704149)) ;
#12349 = CARTESIAN_POINT('Ctrl Pts',(54.63558100691,40.9604252913207,26.6069100286337)) ;
#12350 = CARTESIAN_POINT('Ctrl Pts',(54.551584937626,40.9589933903696,26.6269096646542)) ;
#12351 = CARTESIAN_POINT('Ctrl Pts',(54.4637386379212,40.9583406143964,26.6356835108198)) ;
#12352 = CARTESIAN_POINT('Ctrl Pts',(54.3770957099285,40.9582231658519,26.6372543437853)) ;
#12353 = CARTESIAN_POINT('Ctrl Pts',(54.3673410931221,40.9582099430122,26.6374311946143)) ;
#12354 = CARTESIAN_POINT('Ctrl Pts',(54.357601744153,40.9582035055449,26.6375167608261)) ;
#12355 = CARTESIAN_POINT('Ctrl Pts',(54.3478848524392,40.9582035055449,26.6375167608261)) ;
#12356 = CARTESIAN_POINT('',(53.8421555347741,40.9656750313367,26.5309683918953)) ;
#12357 = CARTESIAN_POINT('Ctrl Pts',(54.3478848524392,40.9582035055449,26.6375167608261)) ;
#12358 = CARTESIAN_POINT('Ctrl Pts',(54.2542634562801,40.9582035055449,26.6375167608261)) ;
#12359 = CARTESIAN_POINT('Ctrl Pts',(54.1585331971118,40.9587531431116,26.6301884706742)) ;
#12360 = CARTESIAN_POINT('Ctrl Pts',(54.0668868671023,40.9601405009254,26.6108805928832)) ;
#12361 = CARTESIAN_POINT('Ctrl Pts',(53.9887808020307,40.9613228838935,26.5944253528428)) ;
#12362 = CARTESIAN_POINT('Ctrl Pts',(53.9123211210366,40.9631399744502,26.5689970708552)) ;
#12363 = CARTESIAN_POINT('Ctrl Pts',(53.8421555347741,40.9656750313367,26.5309683918953)) ;
#12364 = CARTESIAN_POINT('',(53.5615279264748,40.9831482719841,26.2225784301758)) ;
#12365 = CARTESIAN_POINT('Ctrl Pts',(53.8421555347741,40.9656750313367,26.5309683918953)) ;
#12366 = CARTESIAN_POINT('Ctrl Pts',(53.7789593365146,40.9679582798693,26.4967171189199)) ;
#12367 = CARTESIAN_POINT('Ctrl Pts',(53.7221495836717,40.9707165493839,26.4538145079086)) ;
#12368 = CARTESIAN_POINT('Ctrl Pts',(53.6737810081152,40.9738092463041,26.4006816357596)) ;
#12369 = CARTESIAN_POINT('Ctrl Pts',(53.6258672853775,40.9768728598391,26.3480484193559)) ;
#12370 = CARTESIAN_POINT('Ctrl Pts',(53.5888854642734,40.9800818012948,26.2882856508328)) ;
#12371 = CARTESIAN_POINT('Ctrl Pts',(53.5615279264748,40.9831482719841,26.2225784301758)) ;
#12372 = CARTESIAN_POINT('',(53.4774895496666,40.9990558578356,25.6710775136948)) ;
#12373 = CARTESIAN_POINT('Ctrl Pts',(53.5615279264748,40.9831482719841,26.2225784301758)) ;
#12374 = CARTESIAN_POINT('Ctrl Pts',(53.5408779349284,40.9854628895734,26.1729816447871)) ;
#12375 = CARTESIAN_POINT('Ctrl Pts',(53.5253751590079,40.987678182784,26.1198997215806)) ;
#12376 = CARTESIAN_POINT('Ctrl Pts',(53.513696600705,40.9896391569837,26.0664129848815)) ;
#12377 = CARTESIAN_POINT('Ctrl Pts',(53.5076920063279,40.990647402552,26.0389124878081)) ;
#12378 = CARTESIAN_POINT('Ctrl Pts',(53.5026976867563,40.9915884174085,26.0113061709377)) ;
#12379 = CARTESIAN_POINT('Ctrl Pts',(53.4985341824635,40.9924411346845,25.9840120745748)) ;
#12380 = CARTESIAN_POINT('Ctrl Pts',(53.4874089677846,40.9947196630803,25.9110800778353)) ;
#12381 = CARTESIAN_POINT('Ctrl Pts',(53.4814376784056,40.9965384732081,25.8352569009168)) ;
#12382 = CARTESIAN_POINT('Ctrl Pts',(53.4789345818655,40.9978067335497,25.7602369385911)) ;
#12383 = CARTESIAN_POINT('Ctrl Pts',(53.477936122294,40.9983126296096,25.7303122440243)) ;
#12384 = CARTESIAN_POINT('Ctrl Pts',(53.4774895496666,40.9987309260202,25.7005152594796)) ;
#12385 = CARTESIAN_POINT('Ctrl Pts',(53.4774895496666,40.9990558578356,25.6710775136948)) ;
#12386 = CARTESIAN_POINT('',(53.4774895496666,40.960918459348,24.3999998211861)) ;
#12387 = CARTESIAN_POINT('Origin',(53.4774895496666,25.5,25.5)) ;
#12388 = CARTESIAN_POINT('',(53.7686218805611,40.960918459348,24.3999998211861)) ;
#12389 = CARTESIAN_POINT('',(55.25,40.960918459348,24.3999998211861)) ;
#12390 = CARTESIAN_POINT('',(53.7686218805611,40.9990723481228,25.6695769667625)) ;
#12391 = CARTESIAN_POINT('Origin',(53.7686218805611,25.5,25.5)) ;
#12392 = CARTESIAN_POINT('',(53.8218959160149,40.9886898603816,26.0920189261436)) ;
#12393 = CARTESIAN_POINT('Ctrl Pts',(53.7686218805611,40.9990723481228,25.6695769667625)) ;
#12394 = CARTESIAN_POINT('Ctrl Pts',(53.7686218805611,40.9986536207666,25.7078479991484)) ;
#12395 = CARTESIAN_POINT('Ctrl Pts',(53.7693327864037,40.9980612736987,25.747554686281)) ;
#12396 = CARTESIAN_POINT('Ctrl Pts',(53.7711491226713,40.9973239200892,25.7872806686854)) ;
#12397 = CARTESIAN_POINT('Ctrl Pts',(53.7731780641889,40.9965002579853,25.8316566449114)) ;
#12398 = CARTESIAN_POINT('Ctrl Pts',(53.7765880391652,40.9954956560657,25.8760519633279)) ;
#12399 = CARTESIAN_POINT('Ctrl Pts',(53.7819364452524,40.9943499971454,25.9184712247707)) ;
#12400 = CARTESIAN_POINT('Ctrl Pts',(53.7853878563205,40.9936106853179,25.9458450453181)) ;
#12401 = CARTESIAN_POINT('Ctrl Pts',(53.7899552866281,40.9927391021004,25.9748706921076)) ;
#12402 = CARTESIAN_POINT('Ctrl Pts',(53.7961183617569,40.9918055707888,26.0035785313425)) ;
#12403 = CARTESIAN_POINT('Ctrl Pts',(53.8013922531887,40.9910067256209,26.0281445189712)) ;
#12404 = CARTESIAN_POINT('Ctrl Pts',(53.8078364687857,40.9901625181187,26.0524724327561)) ;
#12405 = CARTESIAN_POINT('Ctrl Pts',(53.8157490150832,40.9893170139533,26.0753352441417)) ;
#12406 = CARTESIAN_POINT('Ctrl Pts',(53.817706733993,40.9891078196648,26.0809919514137)) ;
#12407 = CARTESIAN_POINT('Ctrl Pts',(53.819754261106,40.9888985459991,26.0865591905408)) ;
#12408 = CARTESIAN_POINT('Ctrl Pts',(53.8218959160149,40.9886898603816,26.0920189261436)) ;
#12409 = CARTESIAN_POINT('',(54.0049793310463,40.979270509389,26.3013641476631)) ;
#12410 = CARTESIAN_POINT('Ctrl Pts',(53.8218959160149,40.9886898603816,26.0920189261436)) ;
#12411 = CARTESIAN_POINT('Ctrl Pts',(53.8392210714188,40.9870016937733,26.1361855699338)) ;
#12412 = CARTESIAN_POINT('Ctrl Pts',(53.863050596707,40.9852704674679,26.1765182482562)) ;
#12413 = CARTESIAN_POINT('Ctrl Pts',(53.8942812696197,40.9836275207232,26.2122350732055)) ;
#12414 = CARTESIAN_POINT('Ctrl Pts',(53.9258591431538,40.9819663088538,26.2483489726542)) ;
#12415 = CARTESIAN_POINT('Ctrl Pts',(53.9632279991133,40.9804949283934,26.2777130858558)) ;
#12416 = CARTESIAN_POINT('Ctrl Pts',(54.0049793310463,40.979270509389,26.3013641476631)) ;
#12417 = CARTESIAN_POINT('',(54.3223734684289,40.9752885064464,26.3748975038528)) ;
#12418 = CARTESIAN_POINT('Ctrl Pts',(54.0049793310463,40.979270509389,26.3013641476631)) ;
#12419 = CARTESIAN_POINT('Ctrl Pts',(54.0501187277971,40.9779467304179,26.3269344615446)) ;
#12420 = CARTESIAN_POINT('Ctrl Pts',(54.0986649923769,40.9769653080002,26.344797292249)) ;
#12421 = CARTESIAN_POINT('Ctrl Pts',(54.1492147081544,40.9763170829053,26.3565100988152)) ;
#12422 = CARTESIAN_POINT('Ctrl Pts',(54.2057771722795,40.9755917532351,26.3696161112036)) ;
#12423 = CARTESIAN_POINT('Ctrl Pts',(54.2643222776773,40.9752885064464,26.3748975038528)) ;
#12424 = CARTESIAN_POINT('Ctrl Pts',(54.3223734684289,40.9752885064464,26.3748975038528)) ;
#12425 = CARTESIAN_POINT('Ctrl Pts',(54.3223734684289,40.9752885064464,26.3748975038528)) ;
#12426 = CARTESIAN_POINT('Ctrl Pts',(54.3786363553446,40.9752885064464,26.3748975038528)) ;
#12427 = CARTESIAN_POINT('Ctrl Pts',(54.437258969987,40.9754864304333,26.3715512815695)) ;
#12428 = CARTESIAN_POINT('Ctrl Pts',(54.4943479752787,40.9759914778937,26.3624599312309)) ;
#12429 = CARTESIAN_POINT('Ctrl Pts',(54.5295757696573,40.9763031264851,26.3568499504874)) ;
#12430 = CARTESIAN_POINT('Ctrl Pts',(54.564217237808,40.9767317193511,26.3490505124776)) ;
#12431 = CARTESIAN_POINT('Ctrl Pts',(54.5973694346344,40.9773029142982,26.3385073041163)) ;
#12432 = CARTESIAN_POINT('Ctrl Pts',(54.6331824164753,40.9779199531743,26.3271179011285)) ;
#12433 = CARTESIAN_POINT('Ctrl Pts',(54.668007874159,40.9787129882677,26.3122910476793)) ;
#12434 = CARTESIAN_POINT('Ctrl Pts',(54.7002658204309,40.9797004593973,26.2930155656316)) ;
#12435 = CARTESIAN_POINT('Ctrl Pts',(54.7297345351508,40.9806025473594,26.2754067669572)) ;
#12436 = CARTESIAN_POINT('Ctrl Pts',(54.7565994843863,40.9816525638485,26.2543618556874)) ;
#12437 = CARTESIAN_POINT('Ctrl Pts',(54.7800817079842,40.9828316466601,26.2293313384056)) ;
#12438 = CARTESIAN_POINT('',(55.9641196317971,40.9807202883652,24.7271485567093)) ;
#12439 = CARTESIAN_POINT('',(55.9641196317971,40.9609184856404,26.5999998092651)) ;
#12440 = CARTESIAN_POINT('Origin',(55.9641196317971,25.5,25.5)) ;
#12441 = CARTESIAN_POINT('',(55.6834920234978,40.9609184856404,26.5999998092651)) ;
#12442 = CARTESIAN_POINT('',(55.25,40.9609184856404,26.5999998092651)) ;
#12443 = CARTESIAN_POINT('',(55.6834920234978,40.960918459348,24.3999998211861)) ;
#12444 = CARTESIAN_POINT('Origin',(55.6834920234978,25.5,25.5)) ;
#12445 = CARTESIAN_POINT('',(56.1216910667717,40.960918459348,24.3999998211861)) ;
#12446 = CARTESIAN_POINT('',(55.25,40.960918459348,24.3999998211861)) ;
#12447 = CARTESIAN_POINT('',(56.6424276418984,40.99324057365,25.9577079057693)) ;
#12448 = CARTESIAN_POINT('Origin',(56.4894174279709,25.5,25.5)) ;
#12449 = CARTESIAN_POINT('',(56.747475463897,40.9801923016591,26.2833557963371)) ;
#12450 = CARTESIAN_POINT('Ctrl Pts',(56.6424276418984,40.99324057365,25.9577079057693)) ;
#12451 = CARTESIAN_POINT('Ctrl Pts',(56.6483878638642,40.9927086674222,25.9757127316555)) ;
#12452 = CARTESIAN_POINT('Ctrl Pts',(56.6543262857709,40.9921439410553,25.993694115101)) ;
#12453 = CARTESIAN_POINT('Ctrl Pts',(56.6602487671082,40.9915482457722,26.0116790901449)) ;
#12454 = CARTESIAN_POINT('Ctrl Pts',(56.6660136628558,40.9909684007698,26.0291855203464)) ;
#12455 = CARTESIAN_POINT('Ctrl Pts',(56.6717635353025,40.9903592129697,26.0466955789032)) ;
#12456 = CARTESIAN_POINT('Ctrl Pts',(56.6774876311401,40.9897223897193,26.0641888337385)) ;
#12457 = CARTESIAN_POINT('Ctrl Pts',(56.6829741240545,40.9891120005242,26.0809559566915)) ;
#12458 = CARTESIAN_POINT('Ctrl Pts',(56.6884369760154,40.9884762225162,26.0977077546731)) ;
#12459 = CARTESIAN_POINT('Ctrl Pts',(56.69385087,40.987816559134,26.1143817395123)) ;
#12460 = CARTESIAN_POINT('Ctrl Pts',(56.697488469878,40.987373330758,26.1255850038151)) ;
#12461 = CARTESIAN_POINT('Ctrl Pts',(56.7011036475429,40.9869193193124,26.1367522405779)) ;
#12462 = CARTESIAN_POINT('Ctrl Pts',(56.7046842492072,40.9864549808355,26.1478519325859)) ;
#12463 = CARTESIAN_POINT('Ctrl Pts',(56.7088048246254,40.9859206176494,26.1606255171189)) ;
#12464 = CARTESIAN_POINT('Ctrl Pts',(56.7129698449496,40.9853585848336,26.1735891038181)) ;
#12465 = CARTESIAN_POINT('Ctrl Pts',(56.717138316371,40.9847773802594,26.1866350483889)) ;
#12466 = CARTESIAN_POINT('Ctrl Pts',(56.7211924167408,40.9842121222929,26.1993230491842)) ;
#12467 = CARTESIAN_POINT('Ctrl Pts',(56.7252498680784,40.9836287301731,26.2120891938011)) ;
#12468 = CARTESIAN_POINT('Ctrl Pts',(56.7292568099678,40.9830350213146,26.2247891155873)) ;
#12469 = CARTESIAN_POINT('Ctrl Pts',(56.7331081381488,40.9824643697502,26.2369958228523)) ;
#12470 = CARTESIAN_POINT('Ctrl Pts',(56.7369128454569,40.9818841872093,26.2491414678219)) ;
#12471 = CARTESIAN_POINT('Ctrl Pts',(56.7406071105412,40.9813014152283,26.2610529483142)) ;
#12472 = CARTESIAN_POINT('Ctrl Pts',(56.7429478552524,40.9809321616958,26.2686002505048)) ;
#12473 = CARTESIAN_POINT('Ctrl Pts',(56.745243940517,40.9805618685835,26.2760526435616)) ;
#12474 = CARTESIAN_POINT('Ctrl Pts',(56.747475463897,40.9801923016591,26.2833557963371)) ;
#12475 = CARTESIAN_POINT('',(56.8645288534462,40.9940150133522,25.9306956768036)) ;
#12476 = CARTESIAN_POINT('Ctrl Pts',(56.747475463897,40.9801923016591,26.2833557963371)) ;
#12477 = CARTESIAN_POINT('Ctrl Pts',(56.7516296828433,40.9808650039904,26.270062269309)) ;
#12478 = CARTESIAN_POINT('Ctrl Pts',(56.7559705130544,40.9815364551589,26.2563722372977)) ;
#12479 = CARTESIAN_POINT('Ctrl Pts',(56.7604101116033,40.9821985064012,26.2425142185715)) ;
#12480 = CARTESIAN_POINT('Ctrl Pts',(56.7649522311146,40.9828758459922,26.2283361850062)) ;
#12481 = CARTESIAN_POINT('Ctrl Pts',(56.7695978154572,40.9835433465108,26.2139820964589)) ;
#12482 = CARTESIAN_POINT('Ctrl Pts',(56.7742722747122,40.9841922815339,26.1996444922584)) ;
#12483 = CARTESIAN_POINT('Ctrl Pts',(56.7791213439405,40.9848654569067,26.1847713205086)) ;
#12484 = CARTESIAN_POINT('Ctrl Pts',(56.7840015368633,40.9855186538863,26.1699157502043)) ;
#12485 = CARTESIAN_POINT('Ctrl Pts',(56.7888493368058,40.9861421311643,26.1552398169195)) ;
#12486 = CARTESIAN_POINT('Ctrl Pts',(56.7910657916994,40.986427190218,26.1485298568278)) ;
#12487 = CARTESIAN_POINT('Ctrl Pts',(56.7932757361307,40.9867060366793,26.1418567490044)) ;
#12488 = CARTESIAN_POINT('Ctrl Pts',(56.79547434982,40.9869777395263,26.1352326309442)) ;
#12489 = CARTESIAN_POINT('Ctrl Pts',(56.8015533905598,40.9877289823135,26.1169173244634)) ;
#12490 = CARTESIAN_POINT('Ctrl Pts',(56.8077231978965,40.9884516701256,26.0984417037313)) ;
#12491 = CARTESIAN_POINT('Ctrl Pts',(56.8139415434462,40.9891439875036,26.0799085148923)) ;
#12492 = CARTESIAN_POINT('Ctrl Pts',(56.8203227048416,40.9898544319281,26.0608900688751)) ;
#12493 = CARTESIAN_POINT('Ctrl Pts',(56.8267550759624,40.990532894711,26.0418107422561)) ;
#12494 = CARTESIAN_POINT('Ctrl Pts',(56.8332127360803,40.9911774140237,26.0227287647321)) ;
#12495 = CARTESIAN_POINT('Ctrl Pts',(56.8399288127184,40.9918477250992,26.0028831827229)) ;
#12496 = CARTESIAN_POINT('Ctrl Pts',(56.8466722984513,40.9924813217134,25.9830345844242)) ;
#12497 = CARTESIAN_POINT('Ctrl Pts',(56.8534339469647,40.9930759969675,25.9631951372186)) ;
#12498 = CARTESIAN_POINT('Ctrl Pts',(56.8571262434297,40.9934007280348,25.9523615186654)) ;
#12499 = CARTESIAN_POINT('Ctrl Pts',(56.8608242923809,40.9937138532788,25.941529727271)) ;
#12500 = CARTESIAN_POINT('Ctrl Pts',(56.8645288534462,40.9940150133522,25.9306956768036)) ;
#12501 = CARTESIAN_POINT('',(57.3912682123482,40.960918459348,24.3999998211861)) ;
#12502 = CARTESIAN_POINT('Origin',(57.0127388089699,25.5,25.5)) ;
#12503 = CARTESIAN_POINT('',(57.782945830375,40.960918459348,24.3999998211861)) ;
#12504 = CARTESIAN_POINT('',(55.25,40.960918459348,24.3999998211861)) ;
#12505 = CARTESIAN_POINT('',(57.782945830375,40.9609184856404,26.5999998092651)) ;
#12506 = CARTESIAN_POINT('Origin',(57.782945830375,25.5,25.5)) ;
#12507 = CARTESIAN_POINT('',(57.5023188181221,40.9609184856404,26.5999998092651)) ;
#12508 = CARTESIAN_POINT('',(55.25,40.9609184856404,26.5999998092651)) ;
#12509 = CARTESIAN_POINT('',(57.5023188181221,40.9822614389786,24.7586628735065)) ;
#12510 = CARTESIAN_POINT('Origin',(57.5023188181221,25.5,25.5)) ;
#12511 = CARTESIAN_POINT('',(56.8630280084908,40.9609184856404,26.5999998092651)) ;
#12512 = CARTESIAN_POINT('Origin',(57.2449351733355,25.5,25.5)) ;
#12513 = CARTESIAN_POINT('',(56.6004087515175,40.9609184856404,26.5999998092651)) ;
#12514 = CARTESIAN_POINT('',(55.25,40.9609184856404,26.5999998092651)) ;
#12515 = CARTESIAN_POINT('Origin',(56.2266909192151,25.5,25.5)) ;
#12516 = CARTESIAN_POINT('',(58.5933150835335,40.960918459348,24.3999998211861)) ;
#12517 = CARTESIAN_POINT('',(58.5933150835335,40.9609184856404,26.5999998092651)) ;
#12518 = CARTESIAN_POINT('Origin',(58.5933150835335,25.5,25.5)) ;
#12519 = CARTESIAN_POINT('',(58.3021833486855,40.9609184856404,26.5999998092651)) ;
#12520 = CARTESIAN_POINT('',(55.25,40.9609184856404,26.5999998092651)) ;
#12521 = CARTESIAN_POINT('',(58.3021833486855,40.960918459348,24.3999998211861)) ;
#12522 = CARTESIAN_POINT('Origin',(58.3021833486855,25.5,25.5)) ;
#12523 = CARTESIAN_POINT('',(55.25,40.960918459348,24.3999998211861)) ;
#12524 = CARTESIAN_POINT('',(50.9098227806389,40.960918459348,24.3999998211861)) ;
#12525 = CARTESIAN_POINT('',(50.9098227806389,40.9609184856404,26.5999998092651)) ;
#12526 = CARTESIAN_POINT('Origin',(50.9098227806389,25.5,25.5)) ;
#12527 = CARTESIAN_POINT('',(50.6186904497445,40.9609184856404,26.5999998092651)) ;
#12528 = CARTESIAN_POINT('',(55.25,40.9609184856404,26.5999998092651)) ;
#12529 = CARTESIAN_POINT('',(50.6186904497445,40.960918459348,24.3999998211861)) ;
#12530 = CARTESIAN_POINT('Origin',(50.6186904497445,25.5,25.5)) ;
#12531 = CARTESIAN_POINT('',(55.25,40.960918459348,24.3999998211861)) ;
#12532 = CARTESIAN_POINT('Origin',(50.6186904497445,41.5,26.5999998092651)) ;
#12533 = CARTESIAN_POINT('',(50.6186904497445,40.85,26.5999998092651)) ;
#12534 = CARTESIAN_POINT('',(50.6186904497445,41.5,26.5999998092651)) ;
#12535 = CARTESIAN_POINT('',(50.6186904497445,40.85,24.3999998211861)) ;
#12536 = CARTESIAN_POINT('',(50.6186904497445,40.85,26.5999998092651)) ;
#12537 = CARTESIAN_POINT('',(50.6186904497445,41.5,24.3999998211861)) ;
#12538 = CARTESIAN_POINT('Origin',(50.6186904497445,41.5,24.3999998211861)) ;
#12539 = CARTESIAN_POINT('',(50.9098227806389,40.85,24.3999998211861)) ;
#12540 = CARTESIAN_POINT('',(50.6186904497445,40.85,24.3999998211861)) ;
#12541 = CARTESIAN_POINT('',(50.9098227806389,41.5,24.3999998211861)) ;
#12542 = CARTESIAN_POINT('Origin',(50.9098227806389,41.5,24.3999998211861)) ;
#12543 = CARTESIAN_POINT('',(50.9098227806389,40.85,26.5999998092651)) ;
#12544 = CARTESIAN_POINT('',(50.9098227806389,40.85,24.3999998211861)) ;
#12545 = CARTESIAN_POINT('',(50.9098227806389,41.5,26.5999998092651)) ;
#12546 = CARTESIAN_POINT('Origin',(50.9098227806389,41.5,26.5999998092651)) ;
#12547 = CARTESIAN_POINT('',(50.9098227806389,40.85,26.5999998092651)) ;
#12548 = CARTESIAN_POINT('Origin',(53.2966575417668,40.85,25.4999998152256)) ;
#12549 = CARTESIAN_POINT('Origin',(58.3021833486855,41.5,26.5999998092651)) ;
#12550 = CARTESIAN_POINT('',(58.3021833486855,40.85,26.5999998092651)) ;
#12551 = CARTESIAN_POINT('',(58.3021833486855,41.5,26.5999998092651)) ;
#12552 = CARTESIAN_POINT('',(58.3021833486855,40.85,24.3999998211861)) ;
#12553 = CARTESIAN_POINT('',(58.3021833486855,40.85,26.5999998092651)) ;
#12554 = CARTESIAN_POINT('',(58.3021833486855,41.5,24.3999998211861)) ;
#12555 = CARTESIAN_POINT('Origin',(58.3021833486855,41.5,24.3999998211861)) ;
#12556 = CARTESIAN_POINT('',(58.5933150835335,40.85,24.3999998211861)) ;
#12557 = CARTESIAN_POINT('',(58.3021833486855,40.85,24.3999998211861)) ;
#12558 = CARTESIAN_POINT('',(58.5933150835335,41.5,24.3999998211861)) ;
#12559 = CARTESIAN_POINT('Origin',(58.5933150835335,41.5,24.3999998211861)) ;
#12560 = CARTESIAN_POINT('',(58.5933150835335,40.85,26.5999998092651)) ;
#12561 = CARTESIAN_POINT('',(58.5933150835335,40.85,24.3999998211861)) ;
#12562 = CARTESIAN_POINT('',(58.5933150835335,41.5,26.5999998092651)) ;
#12563 = CARTESIAN_POINT('Origin',(58.5933150835335,41.5,26.5999998092651)) ;
#12564 = CARTESIAN_POINT('',(58.5933150835335,40.85,26.5999998092651)) ;
#12565 = CARTESIAN_POINT('Origin',(53.2966575417668,40.85,25.4999998152256)) ;
#12566 = CARTESIAN_POINT('Origin',(57.3912682123482,41.5,24.3999998211861)) ;
#12567 = CARTESIAN_POINT('',(57.3912682123482,40.85,24.3999998211861)) ;
#12568 = CARTESIAN_POINT('',(57.3912682123482,41.5,24.3999998211861)) ;
#12569 = CARTESIAN_POINT('',(57.782945830375,40.85,24.3999998211861)) ;
#12570 = CARTESIAN_POINT('',(57.3912682123482,40.85,24.3999998211861)) ;
#12571 = CARTESIAN_POINT('',(57.782945830375,41.5,24.3999998211861)) ;
#12572 = CARTESIAN_POINT('Origin',(57.782945830375,41.5,24.3999998211861)) ;
#12573 = CARTESIAN_POINT('',(57.782945830375,40.85,26.5999998092651)) ;
#12574 = CARTESIAN_POINT('',(57.782945830375,40.85,24.3999998211861)) ;
#12575 = CARTESIAN_POINT('',(57.782945830375,41.5,26.5999998092651)) ;
#12576 = CARTESIAN_POINT('Origin',(57.782945830375,41.5,26.5999998092651)) ;
#12577 = CARTESIAN_POINT('',(57.5023188181221,40.85,26.5999998092651)) ;
#12578 = CARTESIAN_POINT('',(57.782945830375,40.85,26.5999998092651)) ;
#12579 = CARTESIAN_POINT('',(57.5023188181221,41.5,26.5999998092651)) ;
#12580 = CARTESIAN_POINT('Origin',(57.5023188181221,41.5,26.5999998092651)) ;
#12581 = CARTESIAN_POINT('',(57.5023188181221,40.85,24.7586628735065)) ;
#12582 = CARTESIAN_POINT('',(57.5023188181221,40.85,26.5999998092651)) ;
#12583 = CARTESIAN_POINT('',(57.5023188181221,41.5,24.7586628735065)) ;
#12584 = CARTESIAN_POINT('Origin',(57.5023188181221,41.5,24.7586628735065)) ;
#12585 = CARTESIAN_POINT('',(56.8630280084908,40.85,26.5999998092651)) ;
#12586 = CARTESIAN_POINT('',(57.5023188181221,40.85,24.7586628735065)) ;
#12587 = CARTESIAN_POINT('',(56.8630280084908,41.5,26.5999998092651)) ;
#12588 = CARTESIAN_POINT('Origin',(56.8630280084908,41.5,26.5999998092651)) ;
#12589 = CARTESIAN_POINT('',(56.6004087515175,40.85,26.5999998092651)) ;
#12590 = CARTESIAN_POINT('',(56.8630280084908,40.85,26.5999998092651)) ;
#12591 = CARTESIAN_POINT('',(56.6004087515175,41.5,26.5999998092651)) ;
#12592 = CARTESIAN_POINT('Origin',(56.6004087515175,41.5,26.5999998092651)) ;
#12593 = CARTESIAN_POINT('',(55.9641196317971,40.85,24.7271485567093)) ;
#12594 = CARTESIAN_POINT('',(56.6004087515175,40.85,26.5999998092651)) ;
#12595 = CARTESIAN_POINT('',(55.9641196317971,41.5,24.7271485567093)) ;
#12596 = CARTESIAN_POINT('Origin',(55.9641196317971,41.5,24.7271485567093)) ;
#12597 = CARTESIAN_POINT('',(55.9641196317971,40.85,26.5999998092651)) ;
#12598 = CARTESIAN_POINT('',(55.9641196317971,40.85,24.7271485567093)) ;
#12599 = CARTESIAN_POINT('',(55.9641196317971,41.5,26.5999998092651)) ;
#12600 = CARTESIAN_POINT('Origin',(56.8645288534462,41.5,25.9306956768036)) ;
#12601 = CARTESIAN_POINT('',(56.8645288534462,40.85,25.9306956768036)) ;
#12602 = CARTESIAN_POINT('',(56.8645288534462,41.5,25.9306956768036)) ;
#12603 = CARTESIAN_POINT('',(56.8645288534462,40.85,25.9306956768036)) ;
#12604 = CARTESIAN_POINT('Ctrl Pts',(56.747475463897,41.5,26.2833557963371)) ;
#12605 = CARTESIAN_POINT('Ctrl Pts',(56.747475463897,40.85,26.2833557963371)) ;
#12606 = CARTESIAN_POINT('Ctrl Pts',(56.784992415458,41.5,26.1633013129234)) ;
#12607 = CARTESIAN_POINT('Ctrl Pts',(56.784992415458,40.85,26.1633013129234)) ;
#12608 = CARTESIAN_POINT('Ctrl Pts',(56.8645288534462,41.5,25.9306956768036)) ;
#12609 = CARTESIAN_POINT('Ctrl Pts',(56.8645288534462,40.85,25.9306956768036)) ;
#12610 = CARTESIAN_POINT('',(56.747475463897,40.85,26.2833557963371)) ;
#12611 = CARTESIAN_POINT('',(56.747475463897,41.5,26.2833557963371)) ;
#12612 = CARTESIAN_POINT('Ctrl Pts',(56.747475463897,40.85,26.2833557963371)) ;
#12613 = CARTESIAN_POINT('Ctrl Pts',(56.784992415458,40.85,26.1633013129234)) ;
#12614 = CARTESIAN_POINT('Ctrl Pts',(56.8645288534462,40.85,25.9306956768036)) ;
#12615 = CARTESIAN_POINT('Ctrl Pts',(56.6424276418984,41.5,25.9577079057693)) ;
#12616 = CARTESIAN_POINT('Ctrl Pts',(56.6424276418984,40.85,25.9577079057693)) ;
#12617 = CARTESIAN_POINT('Ctrl Pts',(56.7144604511559,41.5,26.1753068804741)) ;
#12618 = CARTESIAN_POINT('Ctrl Pts',(56.7144604511559,40.85,26.1753068804741)) ;
#12619 = CARTESIAN_POINT('Ctrl Pts',(56.747475463897,41.5,26.2833557963371)) ;
#12620 = CARTESIAN_POINT('Ctrl Pts',(56.747475463897,40.85,26.2833557963371)) ;
#12621 = CARTESIAN_POINT('',(56.6424276418984,40.85,25.9577079057693)) ;
#12622 = CARTESIAN_POINT('',(56.6424276418984,41.5,25.9577079057693)) ;
#12623 = CARTESIAN_POINT('Ctrl Pts',(56.6424276418984,40.85,25.9577079057693)) ;
#12624 = CARTESIAN_POINT('Ctrl Pts',(56.7144604511559,40.85,26.1753068804741)) ;
#12625 = CARTESIAN_POINT('Ctrl Pts',(56.747475463897,40.85,26.2833557963371)) ;
#12626 = CARTESIAN_POINT('Origin',(56.1216910667717,41.5,24.3999998211861)) ;
#12627 = CARTESIAN_POINT('',(56.1216910667717,40.85,24.3999998211861)) ;
#12628 = CARTESIAN_POINT('',(56.1216910667717,41.5,24.3999998211861)) ;
#12629 = CARTESIAN_POINT('',(56.1216910667717,40.85,24.3999998211861)) ;
#12630 = CARTESIAN_POINT('Origin',(55.6834920234978,41.5,24.3999998211861)) ;
#12631 = CARTESIAN_POINT('',(55.6834920234978,40.85,24.3999998211861)) ;
#12632 = CARTESIAN_POINT('',(55.6834920234978,41.5,24.3999998211861)) ;
#12633 = CARTESIAN_POINT('',(55.6834920234978,40.85,24.3999998211861)) ;
#12634 = CARTESIAN_POINT('Origin',(55.6834920234978,41.5,26.5999998092651)) ;
#12635 = CARTESIAN_POINT('',(55.6834920234978,40.85,26.5999998092651)) ;
#12636 = CARTESIAN_POINT('',(55.6834920234978,41.5,26.5999998092651)) ;
#12637 = CARTESIAN_POINT('',(55.6834920234978,40.85,26.5999998092651)) ;
#12638 = CARTESIAN_POINT('Origin',(55.9641196317971,41.5,26.5999998092651)) ;
#12639 = CARTESIAN_POINT('',(55.9641196317971,40.85,26.5999998092651)) ;
#12640 = CARTESIAN_POINT('Origin',(53.2966575417668,40.85,25.4999998152256)) ;
#12641 = CARTESIAN_POINT('Ctrl Pts',(53.5615279264748,41.5,26.2225784301758)) ;
#12642 = CARTESIAN_POINT('Ctrl Pts',(53.5615279264748,40.85,26.2225784301758)) ;
#12643 = CARTESIAN_POINT('Ctrl Pts',(53.4774895496666,41.5,26.0207365393639)) ;
#12644 = CARTESIAN_POINT('Ctrl Pts',(53.4774895496666,40.85,26.0207365393639)) ;
#12645 = CARTESIAN_POINT('Ctrl Pts',(53.4774895496666,41.5,25.6710775136948)) ;
#12646 = CARTESIAN_POINT('Ctrl Pts',(53.4774895496666,40.85,25.6710775136948)) ;
#12647 = CARTESIAN_POINT('',(53.5615279264748,40.85,26.2225784301758)) ;
#12648 = CARTESIAN_POINT('',(53.5615279264748,41.5,26.2225784301758)) ;
#12649 = CARTESIAN_POINT('',(53.4774895496666,40.85,25.6710775136948)) ;
#12650 = CARTESIAN_POINT('Ctrl Pts',(53.5615279264748,40.85,26.2225784301758)) ;
#12651 = CARTESIAN_POINT('Ctrl Pts',(53.4774895496666,40.85,26.0207365393639)) ;
#12652 = CARTESIAN_POINT('Ctrl Pts',(53.4774895496666,40.85,25.6710775136948)) ;
#12653 = CARTESIAN_POINT('',(53.4774895496666,41.5,25.6710775136948)) ;
#12654 = CARTESIAN_POINT('Origin',(53.4774895496666,41.5,25.6710775136948)) ;
#12655 = CARTESIAN_POINT('',(53.4774895496666,40.85,24.3999998211861)) ;
#12656 = CARTESIAN_POINT('',(53.4774895496666,40.85,25.6710775136948)) ;
#12657 = CARTESIAN_POINT('',(53.4774895496666,41.5,24.3999998211861)) ;
#12658 = CARTESIAN_POINT('Origin',(53.4774895496666,41.5,24.3999998211861)) ;
#12659 = CARTESIAN_POINT('',(53.7686218805611,40.85,24.3999998211861)) ;
#12660 = CARTESIAN_POINT('',(53.4774895496666,40.85,24.3999998211861)) ;
#12661 = CARTESIAN_POINT('',(53.7686218805611,41.5,24.3999998211861)) ;
#12662 = CARTESIAN_POINT('Origin',(53.7686218805611,41.5,24.3999998211861)) ;
#12663 = CARTESIAN_POINT('',(53.7686218805611,40.85,25.6695769667625)) ;
#12664 = CARTESIAN_POINT('',(53.7686218805611,40.85,24.3999998211861)) ;
#12665 = CARTESIAN_POINT('',(53.7686218805611,41.5,25.6695769667625)) ;
#12666 = CARTESIAN_POINT('Ctrl Pts',(53.7686218805611,41.5,25.6695769667625)) ;
#12667 = CARTESIAN_POINT('Ctrl Pts',(53.7686218805611,40.85,25.6695769667625)) ;
#12668 = CARTESIAN_POINT('Ctrl Pts',(53.7686218805611,41.5,25.9562070608139)) ;
#12669 = CARTESIAN_POINT('Ctrl Pts',(53.7686218805611,40.85,25.9562070608139)) ;
#12670 = CARTESIAN_POINT('Ctrl Pts',(53.8218959160149,41.5,26.0920189261436)) ;
#12671 = CARTESIAN_POINT('Ctrl Pts',(53.8218959160149,40.85,26.0920189261436)) ;
#12672 = CARTESIAN_POINT('',(53.8218959160149,40.85,26.0920189261436)) ;
#12673 = CARTESIAN_POINT('Ctrl Pts',(53.7686218805611,40.85,25.6695769667625)) ;
#12674 = CARTESIAN_POINT('Ctrl Pts',(53.7686218805611,40.85,25.9562070608139)) ;
#12675 = CARTESIAN_POINT('Ctrl Pts',(53.8218959160149,40.85,26.0920189261436)) ;
#12676 = CARTESIAN_POINT('',(53.8218959160149,41.5,26.0920189261436)) ;
#12677 = CARTESIAN_POINT('Ctrl Pts',(53.8218959160149,41.5,26.0920189261436)) ;
#12678 = CARTESIAN_POINT('Ctrl Pts',(53.8218959160149,40.85,26.0920189261436)) ;
#12679 = CARTESIAN_POINT('Ctrl Pts',(53.8751705475152,41.5,26.2278307914734)) ;
#12680 = CARTESIAN_POINT('Ctrl Pts',(53.8751705475152,40.85,26.2278307914734)) ;
#12681 = CARTESIAN_POINT('Ctrl Pts',(54.0049793310463,41.5,26.3013641476631)) ;
#12682 = CARTESIAN_POINT('Ctrl Pts',(54.0049793310463,40.85,26.3013641476631)) ;
#12683 = CARTESIAN_POINT('',(54.0049793310463,40.85,26.3013641476631)) ;
#12684 = CARTESIAN_POINT('Ctrl Pts',(53.8218959160149,40.85,26.0920189261436)) ;
#12685 = CARTESIAN_POINT('Ctrl Pts',(53.8751705475152,40.85,26.2278307914734)) ;
#12686 = CARTESIAN_POINT('Ctrl Pts',(54.0049793310463,40.85,26.3013641476631)) ;
#12687 = CARTESIAN_POINT('',(54.0049793310463,41.5,26.3013641476631)) ;
#12688 = CARTESIAN_POINT('Ctrl Pts',(54.0049793310463,41.5,26.3013641476631)) ;
#12689 = CARTESIAN_POINT('Ctrl Pts',(54.0049793310463,40.85,26.3013641476631)) ;
#12690 = CARTESIAN_POINT('Ctrl Pts',(54.1347881145775,41.5,26.3748975038528)) ;
#12691 = CARTESIAN_POINT('Ctrl Pts',(54.1347881145775,40.85,26.3748975038528)) ;
#12692 = CARTESIAN_POINT('Ctrl Pts',(54.3223734684289,41.5,26.3748975038528)) ;
#12693 = CARTESIAN_POINT('Ctrl Pts',(54.3223734684289,40.85,26.3748975038528)) ;
#12694 = CARTESIAN_POINT('',(54.3223734684289,40.85,26.3748975038528)) ;
#12695 = CARTESIAN_POINT('Ctrl Pts',(54.0049793310463,40.85,26.3013641476631)) ;
#12696 = CARTESIAN_POINT('Ctrl Pts',(54.1347881145775,40.85,26.3748975038528)) ;
#12697 = CARTESIAN_POINT('Ctrl Pts',(54.3223734684289,40.85,26.3748975038528)) ;
#12698 = CARTESIAN_POINT('',(54.3223734684289,41.5,26.3748975038528)) ;
#12699 = CARTESIAN_POINT('Ctrl Pts',(54.3223734684289,41.5,26.3748975038528)) ;
#12700 = CARTESIAN_POINT('Ctrl Pts',(54.3223734684289,40.85,26.3748975038528)) ;
#12701 = CARTESIAN_POINT('Ctrl Pts',(54.6435197182,41.5,26.3748975038528)) ;
#12702 = CARTESIAN_POINT('Ctrl Pts',(54.6435197182,40.85,26.3748975038528)) ;
#12703 = CARTESIAN_POINT('Ctrl Pts',(54.7800817079842,41.5,26.2293313384056)) ;
#12704 = CARTESIAN_POINT('Ctrl Pts',(54.7800817079842,40.85,26.2293313384056)) ;
#12705 = CARTESIAN_POINT('',(54.7800817079842,40.85,26.2293313384056)) ;
#12706 = CARTESIAN_POINT('Ctrl Pts',(54.3223734684289,40.85,26.3748975038528)) ;
#12707 = CARTESIAN_POINT('Ctrl Pts',(54.6435197182,40.85,26.3748975038528)) ;
#12708 = CARTESIAN_POINT('Ctrl Pts',(54.7800817079842,40.85,26.2293313384056)) ;
#12709 = CARTESIAN_POINT('',(54.7800817079842,41.5,26.2293313384056)) ;
#12710 = CARTESIAN_POINT('Ctrl Pts',(54.7800817079842,41.5,26.2293313384056)) ;
#12711 = CARTESIAN_POINT('Ctrl Pts',(54.7800817079842,40.85,26.2293313384056)) ;
#12712 = CARTESIAN_POINT('Ctrl Pts',(54.9166436977684,41.5,26.0837651729584)) ;
#12713 = CARTESIAN_POINT('Ctrl Pts',(54.9166436977684,40.85,26.0837651729584)) ;
#12714 = CARTESIAN_POINT('Ctrl Pts',(54.9166436977684,41.5,25.6695769667625)) ;
#12715 = CARTESIAN_POINT('Ctrl Pts',(54.9166436977684,40.85,25.6695769667625)) ;
#12716 = CARTESIAN_POINT('',(54.9166436977684,40.85,25.6695769667625)) ;
#12717 = CARTESIAN_POINT('Ctrl Pts',(54.7800817079842,40.85,26.2293313384056)) ;
#12718 = CARTESIAN_POINT('Ctrl Pts',(54.9166436977684,40.85,26.0837651729584)) ;
#12719 = CARTESIAN_POINT('Ctrl Pts',(54.9166436977684,40.85,25.6695769667625)) ;
#12720 = CARTESIAN_POINT('',(54.9166436977684,41.5,25.6695769667625)) ;
#12721 = CARTESIAN_POINT('Ctrl Pts',(53.8421555347741,41.5,26.5309683918953)) ;
#12722 = CARTESIAN_POINT('Ctrl Pts',(53.8421555347741,40.85,26.5309683918953)) ;
#12723 = CARTESIAN_POINT('Ctrl Pts',(53.6455657072365,41.5,26.4244200229645)) ;
#12724 = CARTESIAN_POINT('Ctrl Pts',(53.6455657072365,40.85,26.4244200229645)) ;
#12725 = CARTESIAN_POINT('Ctrl Pts',(53.5615279264748,41.5,26.2225784301758)) ;
#12726 = CARTESIAN_POINT('Ctrl Pts',(53.5615279264748,40.85,26.2225784301758)) ;
#12727 = CARTESIAN_POINT('',(53.8421555347741,40.85,26.5309683918953)) ;
#12728 = CARTESIAN_POINT('',(53.8421555347741,41.5,26.5309683918953)) ;
#12729 = CARTESIAN_POINT('Ctrl Pts',(53.8421555347741,40.85,26.5309683918953)) ;
#12730 = CARTESIAN_POINT('Ctrl Pts',(53.6455657072365,40.85,26.4244200229645)) ;
#12731 = CARTESIAN_POINT('Ctrl Pts',(53.5615279264748,40.85,26.2225784301758)) ;
#12732 = CARTESIAN_POINT('Ctrl Pts',(54.3478848524392,41.5,26.6375167608261)) ;
#12733 = CARTESIAN_POINT('Ctrl Pts',(54.3478848524392,40.85,26.6375167608261)) ;
#12734 = CARTESIAN_POINT('Ctrl Pts',(54.0387447662652,41.5,26.6375167608261)) ;
#12735 = CARTESIAN_POINT('Ctrl Pts',(54.0387447662652,40.85,26.6375167608261)) ;
#12736 = CARTESIAN_POINT('Ctrl Pts',(53.8421555347741,41.5,26.5309683918953)) ;
#12737 = CARTESIAN_POINT('Ctrl Pts',(53.8421555347741,40.85,26.5309683918953)) ;
#12738 = CARTESIAN_POINT('',(54.3478848524392,40.85,26.6375167608261)) ;
#12739 = CARTESIAN_POINT('',(54.3478848524392,41.5,26.6375167608261)) ;
#12740 = CARTESIAN_POINT('Ctrl Pts',(54.3478848524392,40.85,26.6375167608261)) ;
#12741 = CARTESIAN_POINT('Ctrl Pts',(54.0387447662652,40.85,26.6375167608261)) ;
#12742 = CARTESIAN_POINT('Ctrl Pts',(53.8421555347741,40.85,26.5309683918953)) ;
#12743 = CARTESIAN_POINT('Ctrl Pts',(54.8618688173592,41.5,26.5152113080025)) ;
#12744 = CARTESIAN_POINT('Ctrl Pts',(54.8618688173592,40.85,26.5152113080025)) ;
#12745 = CARTESIAN_POINT('Ctrl Pts',(54.6660300083458,41.5,26.6375167608261)) ;
#12746 = CARTESIAN_POINT('Ctrl Pts',(54.6660300083458,40.85,26.6375167608261)) ;
#12747 = CARTESIAN_POINT('Ctrl Pts',(54.3478848524392,41.5,26.6375167608261)) ;
#12748 = CARTESIAN_POINT('Ctrl Pts',(54.3478848524392,40.85,26.6375167608261)) ;
#12749 = CARTESIAN_POINT('',(54.8618688173592,40.85,26.5152113080025)) ;
#12750 = CARTESIAN_POINT('',(54.8618688173592,41.5,26.5152113080025)) ;
#12751 = CARTESIAN_POINT('Ctrl Pts',(54.8618688173592,40.85,26.5152113080025)) ;
#12752 = CARTESIAN_POINT('Ctrl Pts',(54.6660300083458,40.85,26.6375167608261)) ;
#12753 = CARTESIAN_POINT('Ctrl Pts',(54.3478848524392,40.85,26.6375167608261)) ;
#12754 = CARTESIAN_POINT('Ctrl Pts',(55.132742125541,41.5,26.1978168725967)) ;
#12755 = CARTESIAN_POINT('Ctrl Pts',(55.132742125541,40.85,26.1978168725967)) ;
#12756 = CARTESIAN_POINT('Ctrl Pts',(55.0577076263726,41.5,26.3929055571556)) ;
#12757 = CARTESIAN_POINT('Ctrl Pts',(55.0577076263726,40.85,26.3929055571556)) ;
#12758 = CARTESIAN_POINT('Ctrl Pts',(54.8618688173592,41.5,26.5152113080025)) ;
#12759 = CARTESIAN_POINT('Ctrl Pts',(54.8618688173592,40.85,26.5152113080025)) ;
#12760 = CARTESIAN_POINT('',(55.132742125541,40.85,26.1978168725967)) ;
#12761 = CARTESIAN_POINT('',(55.132742125541,41.5,26.1978168725967)) ;
#12762 = CARTESIAN_POINT('Ctrl Pts',(55.132742125541,40.85,26.1978168725967)) ;
#12763 = CARTESIAN_POINT('Ctrl Pts',(55.0577076263726,40.85,26.3929055571556)) ;
#12764 = CARTESIAN_POINT('Ctrl Pts',(54.8618688173592,40.85,26.5152113080025)) ;
#12765 = CARTESIAN_POINT('Ctrl Pts',(55.2077760286629,41.5,25.6710775136948)) ;
#12766 = CARTESIAN_POINT('Ctrl Pts',(55.2077760286629,40.85,25.6710775136948)) ;
#12767 = CARTESIAN_POINT('Ctrl Pts',(55.2077760286629,41.5,26.0027281880379)) ;
#12768 = CARTESIAN_POINT('Ctrl Pts',(55.2077760286629,40.85,26.0027281880379)) ;
#12769 = CARTESIAN_POINT('Ctrl Pts',(55.132742125541,41.5,26.1978168725967)) ;
#12770 = CARTESIAN_POINT('Ctrl Pts',(55.132742125541,40.85,26.1978168725967)) ;
#12771 = CARTESIAN_POINT('',(55.2077760286629,40.85,25.6710775136948)) ;
#12772 = CARTESIAN_POINT('',(55.2077760286629,41.5,25.6710775136948)) ;
#12773 = CARTESIAN_POINT('Ctrl Pts',(55.2077760286629,40.85,25.6710775136948)) ;
#12774 = CARTESIAN_POINT('Ctrl Pts',(55.2077760286629,40.85,26.0027281880379)) ;
#12775 = CARTESIAN_POINT('Ctrl Pts',(55.132742125541,40.85,26.1978168725967)) ;
#12776 = CARTESIAN_POINT('Origin',(55.2077760286629,41.5,24.3999998211861)) ;
#12777 = CARTESIAN_POINT('',(55.2077760286629,40.85,24.3999998211861)) ;
#12778 = CARTESIAN_POINT('',(55.2077760286629,41.5,24.3999998211861)) ;
#12779 = CARTESIAN_POINT('',(55.2077760286629,40.85,24.3999998211861)) ;
#12780 = CARTESIAN_POINT('Origin',(54.9166436977684,41.5,24.3999998211861)) ;
#12781 = CARTESIAN_POINT('',(54.9166436977684,40.85,24.3999998211861)) ;
#12782 = CARTESIAN_POINT('',(54.9166436977684,41.5,24.3999998211861)) ;
#12783 = CARTESIAN_POINT('',(54.9166436977684,40.85,24.3999998211861)) ;
#12784 = CARTESIAN_POINT('Origin',(54.9166436977684,41.5,25.6695769667625)) ;
#12785 = CARTESIAN_POINT('',(54.9166436977684,40.85,25.6695769667625)) ;
#12786 = CARTESIAN_POINT('Origin',(53.2966575417668,40.85,25.4999998152256)) ;
#12787 = CARTESIAN_POINT('Ctrl Pts',(52.1824010200799,41.5,24.3624828696251)) ;
#12788 = CARTESIAN_POINT('Ctrl Pts',(52.1824010200799,40.85,24.3624828696251)) ;
#12789 = CARTESIAN_POINT('Ctrl Pts',(52.4270125217736,41.5,24.3624828696251)) ;
#12790 = CARTESIAN_POINT('Ctrl Pts',(52.4270125217736,40.85,24.3624828696251)) ;
#12791 = CARTESIAN_POINT('Ctrl Pts',(52.6138474531472,41.5,24.4412685871124)) ;
#12792 = CARTESIAN_POINT('Ctrl Pts',(52.6138474531472,40.85,24.4412685871124)) ;
#12793 = CARTESIAN_POINT('',(52.1824010200799,40.85,24.3624828696251)) ;
#12794 = CARTESIAN_POINT('',(52.1824010200799,41.5,24.3624828696251)) ;
#12795 = CARTESIAN_POINT('',(52.6138474531472,40.85,24.4412685871124)) ;
#12796 = CARTESIAN_POINT('Ctrl Pts',(52.1824010200799,40.85,24.3624828696251)) ;
#12797 = CARTESIAN_POINT('Ctrl Pts',(52.4270125217736,40.85,24.3624828696251)) ;
#12798 = CARTESIAN_POINT('Ctrl Pts',(52.6138474531472,40.85,24.4412685871124)) ;
#12799 = CARTESIAN_POINT('',(52.6138474531472,41.5,24.4412685871124)) ;
#12800 = CARTESIAN_POINT('Ctrl Pts',(52.6138474531472,41.5,24.4412685871124)) ;
#12801 = CARTESIAN_POINT('Ctrl Pts',(52.6138474531472,40.85,24.4412685871124)) ;
#12802 = CARTESIAN_POINT('Ctrl Pts',(52.8006823845208,41.5,24.5200544536114)) ;
#12803 = CARTESIAN_POINT('Ctrl Pts',(52.8006823845208,40.85,24.5200544536114)) ;
#12804 = CARTESIAN_POINT('Ctrl Pts',(52.901227671653,41.5,24.6731239497662)) ;
#12805 = CARTESIAN_POINT('Ctrl Pts',(52.901227671653,40.85,24.6731239497662)) ;
#12806 = CARTESIAN_POINT('',(52.901227671653,40.85,24.6731239497662)) ;
#12807 = CARTESIAN_POINT('Ctrl Pts',(52.6138474531472,40.85,24.4412685871124)) ;
#12808 = CARTESIAN_POINT('Ctrl Pts',(52.8006823845208,40.85,24.5200544536114)) ;
#12809 = CARTESIAN_POINT('Ctrl Pts',(52.901227671653,40.85,24.6731239497662)) ;
#12810 = CARTESIAN_POINT('',(52.901227671653,41.5,24.6731239497662)) ;
#12811 = CARTESIAN_POINT('Ctrl Pts',(52.901227671653,41.5,24.6731239497662)) ;
#12812 = CARTESIAN_POINT('Ctrl Pts',(52.901227671653,40.85,24.6731239497662)) ;
#12813 = CARTESIAN_POINT('Ctrl Pts',(53.0017735548317,41.5,24.8261935949326)) ;
#12814 = CARTESIAN_POINT('Ctrl Pts',(53.0017735548317,40.85,24.8261935949326)) ;
#12815 = CARTESIAN_POINT('Ctrl Pts',(53.0092771835625,41.5,25.0197815835476)) ;
#12816 = CARTESIAN_POINT('Ctrl Pts',(53.0092771835625,40.85,25.0197815835476)) ;
#12817 = CARTESIAN_POINT('',(53.0092771835625,40.85,25.0197815835476)) ;
#12818 = CARTESIAN_POINT('Ctrl Pts',(52.901227671653,40.85,24.6731239497662)) ;
#12819 = CARTESIAN_POINT('Ctrl Pts',(53.0017735548317,40.85,24.8261935949326)) ;
#12820 = CARTESIAN_POINT('Ctrl Pts',(53.0092771835625,40.85,25.0197815835476)) ;
#12821 = CARTESIAN_POINT('',(53.0092771835625,41.5,25.0197815835476)) ;
#12822 = CARTESIAN_POINT('Origin',(53.0092771835625,41.5,25.0197815835476)) ;
#12823 = CARTESIAN_POINT('',(52.7301501221955,40.85,25.0407911777496)) ;
#12824 = CARTESIAN_POINT('',(53.0092771835625,40.85,25.0197815835476)) ;
#12825 = CARTESIAN_POINT('',(52.7301501221955,41.5,25.0407911777496)) ;
#12826 = CARTESIAN_POINT('Ctrl Pts',(52.7301501221955,41.5,25.0407911777496)) ;
#12827 = CARTESIAN_POINT('Ctrl Pts',(52.7301501221955,40.85,25.0407911777496)) ;
#12828 = CARTESIAN_POINT('Ctrl Pts',(52.7076398320496,41.5,24.8321963787079)) ;
#12829 = CARTESIAN_POINT('Ctrl Pts',(52.7076398320496,40.85,24.8321963787079)) ;
#12830 = CARTESIAN_POINT('Ctrl Pts',(52.5778307504952,41.5,24.7256478607655)) ;
#12831 = CARTESIAN_POINT('Ctrl Pts',(52.5778307504952,40.85,24.7256478607655)) ;
#12832 = CARTESIAN_POINT('',(52.5778307504952,40.85,24.7256478607655)) ;
#12833 = CARTESIAN_POINT('Ctrl Pts',(52.7301501221955,40.85,25.0407911777496)) ;
#12834 = CARTESIAN_POINT('Ctrl Pts',(52.7076398320496,40.85,24.8321963787079)) ;
#12835 = CARTESIAN_POINT('Ctrl Pts',(52.5778307504952,40.85,24.7256478607655)) ;
#12836 = CARTESIAN_POINT('',(52.5778307504952,41.5,24.7256478607655)) ;
#12837 = CARTESIAN_POINT('Ctrl Pts',(52.5778307504952,41.5,24.7256478607655)) ;
#12838 = CARTESIAN_POINT('Ctrl Pts',(52.5778307504952,40.85,24.7256478607655)) ;
#12839 = CARTESIAN_POINT('Ctrl Pts',(52.448021966964,41.5,24.6190994918346)) ;
#12840 = CARTESIAN_POINT('Ctrl Pts',(52.448021966964,40.85,24.6190994918346)) ;
#12841 = CARTESIAN_POINT('Ctrl Pts',(52.1944065876305,41.5,24.6190994918346)) ;
#12842 = CARTESIAN_POINT('Ctrl Pts',(52.1944065876305,40.85,24.6190994918346)) ;
#12843 = CARTESIAN_POINT('',(52.1944065876305,40.85,24.6190994918346)) ;
#12844 = CARTESIAN_POINT('Ctrl Pts',(52.5778307504952,40.85,24.7256478607655)) ;
#12845 = CARTESIAN_POINT('Ctrl Pts',(52.448021966964,40.85,24.6190994918346)) ;
#12846 = CARTESIAN_POINT('Ctrl Pts',(52.1944065876305,40.85,24.6190994918346)) ;
#12847 = CARTESIAN_POINT('',(52.1944065876305,41.5,24.6190994918346)) ;
#12848 = CARTESIAN_POINT('Ctrl Pts',(52.1944065876305,41.5,24.6190994918346)) ;
#12849 = CARTESIAN_POINT('Ctrl Pts',(52.1944065876305,40.85,24.6190994918346)) ;
#12850 = CARTESIAN_POINT('Ctrl Pts',(51.9302864857018,41.5,24.6190994918346)) ;
#12851 = CARTESIAN_POINT('Ctrl Pts',(51.9302864857018,40.85,24.6190994918346)) ;
#12852 = CARTESIAN_POINT('Ctrl Pts',(51.8094815798104,41.5,24.7158934116364)) ;
#12853 = CARTESIAN_POINT('Ctrl Pts',(51.8094815798104,40.85,24.7158934116364)) ;
#12854 = CARTESIAN_POINT('',(51.8094815798104,40.85,24.7158934116364)) ;
#12855 = CARTESIAN_POINT('Ctrl Pts',(52.1944065876305,40.85,24.6190994918346)) ;
#12856 = CARTESIAN_POINT('Ctrl Pts',(51.9302864857018,40.85,24.6190994918346)) ;
#12857 = CARTESIAN_POINT('Ctrl Pts',(51.8094815798104,40.85,24.7158934116364)) ;
#12858 = CARTESIAN_POINT('',(51.8094815798104,41.5,24.7158934116364)) ;
#12859 = CARTESIAN_POINT('Ctrl Pts',(51.8094815798104,41.5,24.7158934116364)) ;
#12860 = CARTESIAN_POINT('Ctrl Pts',(51.8094815798104,40.85,24.7158934116364)) ;
#12861 = CARTESIAN_POINT('Ctrl Pts',(51.688676673919,41.5,24.8126874804497)) ;
#12862 = CARTESIAN_POINT('Ctrl Pts',(51.688676673919,40.85,24.8126874804497)) ;
#12863 = CARTESIAN_POINT('Ctrl Pts',(51.688676673919,41.5,24.9492494702339)) ;
#12864 = CARTESIAN_POINT('Ctrl Pts',(51.688676673919,40.85,24.9492494702339)) ;
#12865 = CARTESIAN_POINT('',(51.688676673919,40.85,24.9492494702339)) ;
#12866 = CARTESIAN_POINT('Ctrl Pts',(51.8094815798104,40.85,24.7158934116364)) ;
#12867 = CARTESIAN_POINT('Ctrl Pts',(51.688676673919,40.85,24.8126874804497)) ;
#12868 = CARTESIAN_POINT('Ctrl Pts',(51.688676673919,40.85,24.9492494702339)) ;
#12869 = CARTESIAN_POINT('',(51.688676673919,41.5,24.9492494702339)) ;
#12870 = CARTESIAN_POINT('Ctrl Pts',(51.688676673919,41.5,24.9492494702339)) ;
#12871 = CARTESIAN_POINT('Ctrl Pts',(51.688676673919,40.85,24.9492494702339)) ;
#12872 = CARTESIAN_POINT('Ctrl Pts',(51.688676673919,41.5,25.0678034067154)) ;
#12873 = CARTESIAN_POINT('Ctrl Pts',(51.688676673919,40.85,25.0678034067154)) ;
#12874 = CARTESIAN_POINT('Ctrl Pts',(51.7742155976593,41.5,25.1443381547928)) ;
#12875 = CARTESIAN_POINT('Ctrl Pts',(51.7742155976593,40.85,25.1443381547928)) ;
#12876 = CARTESIAN_POINT('',(51.7742155976593,40.85,25.1443381547928)) ;
#12877 = CARTESIAN_POINT('Ctrl Pts',(51.688676673919,40.85,24.9492494702339)) ;
#12878 = CARTESIAN_POINT('Ctrl Pts',(51.688676673919,40.85,25.0678034067154)) ;
#12879 = CARTESIAN_POINT('Ctrl Pts',(51.7742155976593,40.85,25.1443381547928)) ;
#12880 = CARTESIAN_POINT('',(51.7742155976593,41.5,25.1443381547928)) ;
#12881 = CARTESIAN_POINT('Ctrl Pts',(51.7742155976593,41.5,25.1443381547928)) ;
#12882 = CARTESIAN_POINT('Ctrl Pts',(51.7742155976593,40.85,25.1443381547928)) ;
#12883 = CARTESIAN_POINT('Ctrl Pts',(51.8582536764443,41.5,25.2208730518818)) ;
#12884 = CARTESIAN_POINT('Ctrl Pts',(51.8582536764443,40.85,25.2208730518818)) ;
#12885 = CARTESIAN_POINT('Ctrl Pts',(52.213165063411,41.5,25.301159465313)) ;
#12886 = CARTESIAN_POINT('Ctrl Pts',(52.213165063411,40.85,25.301159465313)) ;
#12887 = CARTESIAN_POINT('',(52.213165063411,40.85,25.301159465313)) ;
#12888 = CARTESIAN_POINT('Ctrl Pts',(51.7742155976593,40.85,25.1443381547928)) ;
#12889 = CARTESIAN_POINT('Ctrl Pts',(51.8582536764443,40.85,25.2208730518818)) ;
#12890 = CARTESIAN_POINT('Ctrl Pts',(52.213165063411,40.85,25.301159465313)) ;
#12891 = CARTESIAN_POINT('',(52.213165063411,41.5,25.301159465313)) ;
#12892 = CARTESIAN_POINT('Ctrl Pts',(52.213165063411,41.5,25.301159465313)) ;
#12893 = CARTESIAN_POINT('Ctrl Pts',(52.213165063411,40.85,25.301159465313)) ;
#12894 = CARTESIAN_POINT('Ctrl Pts',(52.5680764503777,41.5,25.3814460277557)) ;
#12895 = CARTESIAN_POINT('Ctrl Pts',(52.5680764503777,40.85,25.3814460277557)) ;
#12896 = CARTESIAN_POINT('Ctrl Pts',(52.7001365013421,41.5,25.4414732694626)) ;
#12897 = CARTESIAN_POINT('Ctrl Pts',(52.7001365013421,40.85,25.4414732694626)) ;
#12898 = CARTESIAN_POINT('',(52.7001365013421,40.85,25.4414732694626)) ;
#12899 = CARTESIAN_POINT('Ctrl Pts',(52.213165063411,40.85,25.301159465313)) ;
#12900 = CARTESIAN_POINT('Ctrl Pts',(52.5680764503777,40.85,25.3814460277557)) ;
#12901 = CARTESIAN_POINT('Ctrl Pts',(52.7001365013421,40.85,25.4414732694626)) ;
#12902 = CARTESIAN_POINT('',(52.7001365013421,41.5,25.4414732694626)) ;
#12903 = CARTESIAN_POINT('Ctrl Pts',(52.7001365013421,41.5,25.4414732694626)) ;
#12904 = CARTESIAN_POINT('Ctrl Pts',(52.7001365013421,40.85,25.4414732694626)) ;
#12905 = CARTESIAN_POINT('Ctrl Pts',(52.8922237940133,41.5,25.530013436079)) ;
#12906 = CARTESIAN_POINT('Ctrl Pts',(52.8922237940133,40.85,25.530013436079)) ;
#12907 = CARTESIAN_POINT('Ctrl Pts',(52.9837652035058,41.5,25.6658251523972)) ;
#12908 = CARTESIAN_POINT('Ctrl Pts',(52.9837652035058,40.85,25.6658251523972)) ;
#12909 = CARTESIAN_POINT('',(52.9837652035058,40.85,25.6658251523972)) ;
#12910 = CARTESIAN_POINT('Ctrl Pts',(52.7001365013421,40.85,25.4414732694626)) ;
#12911 = CARTESIAN_POINT('Ctrl Pts',(52.8922237940133,40.85,25.530013436079)) ;
#12912 = CARTESIAN_POINT('Ctrl Pts',(52.9837652035058,40.85,25.6658251523972)) ;
#12913 = CARTESIAN_POINT('',(52.9837652035058,41.5,25.6658251523972)) ;
#12914 = CARTESIAN_POINT('Ctrl Pts',(52.9837652035058,41.5,25.6658251523972)) ;
#12915 = CARTESIAN_POINT('Ctrl Pts',(52.9837652035058,40.85,25.6658251523972)) ;
#12916 = CARTESIAN_POINT('Ctrl Pts',(53.0753072090447,41.5,25.8016368687153)) ;
#12917 = CARTESIAN_POINT('Ctrl Pts',(53.0753072090447,40.85,25.8016368687153)) ;
#12918 = CARTESIAN_POINT('Ctrl Pts',(53.0753072090447,41.5,25.9787173509598)) ;
#12919 = CARTESIAN_POINT('Ctrl Pts',(53.0753072090447,40.85,25.9787173509598)) ;
#12920 = CARTESIAN_POINT('',(53.0753072090447,40.85,25.9787173509598)) ;
#12921 = CARTESIAN_POINT('Ctrl Pts',(52.9837652035058,40.85,25.6658251523972)) ;
#12922 = CARTESIAN_POINT('Ctrl Pts',(53.0753072090447,40.85,25.8016368687153)) ;
#12923 = CARTESIAN_POINT('Ctrl Pts',(53.0753072090447,40.85,25.9787173509598)) ;
#12924 = CARTESIAN_POINT('',(53.0753072090447,41.5,25.9787173509598)) ;
#12925 = CARTESIAN_POINT('Ctrl Pts',(53.0753072090447,41.5,25.9787173509598)) ;
#12926 = CARTESIAN_POINT('Ctrl Pts',(53.0753072090447,40.85,25.9787173509598)) ;
#12927 = CARTESIAN_POINT('Ctrl Pts',(53.0753072090447,41.5,26.1542971372604)) ;
#12928 = CARTESIAN_POINT('Ctrl Pts',(53.0753072090447,40.85,26.1542971372604)) ;
#12929 = CARTESIAN_POINT('Ctrl Pts',(52.974761325866,41.5,26.3096179008484)) ;
#12930 = CARTESIAN_POINT('Ctrl Pts',(52.974761325866,40.85,26.3096179008484)) ;
#12931 = CARTESIAN_POINT('',(52.974761325866,40.85,26.3096179008484)) ;
#12932 = CARTESIAN_POINT('Ctrl Pts',(53.0753072090447,40.85,25.9787173509598)) ;
#12933 = CARTESIAN_POINT('Ctrl Pts',(53.0753072090447,40.85,26.1542971372604)) ;
#12934 = CARTESIAN_POINT('Ctrl Pts',(52.974761325866,40.85,26.3096179008484)) ;
#12935 = CARTESIAN_POINT('',(52.974761325866,41.5,26.3096179008484)) ;
#12936 = CARTESIAN_POINT('Ctrl Pts',(52.974761325866,41.5,26.3096179008484)) ;
#12937 = CARTESIAN_POINT('Ctrl Pts',(52.974761325866,40.85,26.3096179008484)) ;
#12938 = CARTESIAN_POINT('Ctrl Pts',(52.8742154426873,41.5,26.4649383664131)) ;
#12939 = CARTESIAN_POINT('Ctrl Pts',(52.8742154426873,40.85,26.4649383664131)) ;
#12940 = CARTESIAN_POINT('Ctrl Pts',(52.6858799643815,41.5,26.5512277126312)) ;
#12941 = CARTESIAN_POINT('Ctrl Pts',(52.6858799643815,40.85,26.5512277126312)) ;
#12942 = CARTESIAN_POINT('',(52.6858799643815,40.85,26.5512277126312)) ;
#12943 = CARTESIAN_POINT('Ctrl Pts',(52.974761325866,40.85,26.3096179008484)) ;
#12944 = CARTESIAN_POINT('Ctrl Pts',(52.8742154426873,40.85,26.4649383664131)) ;
#12945 = CARTESIAN_POINT('Ctrl Pts',(52.6858799643815,40.85,26.5512277126312)) ;
#12946 = CARTESIAN_POINT('',(52.6858799643815,41.5,26.5512277126312)) ;
#12947 = CARTESIAN_POINT('Ctrl Pts',(52.6858799643815,41.5,26.5512277126312)) ;
#12948 = CARTESIAN_POINT('Ctrl Pts',(52.6858799643815,40.85,26.5512277126312)) ;
#12949 = CARTESIAN_POINT('Ctrl Pts',(52.4975444860756,41.5,26.6375167608261)) ;
#12950 = CARTESIAN_POINT('Ctrl Pts',(52.4975444860756,40.85,26.6375167608261)) ;
#12951 = CARTESIAN_POINT('Ctrl Pts',(52.2619374580681,41.5,26.6375167608261)) ;
#12952 = CARTESIAN_POINT('Ctrl Pts',(52.2619374580681,40.85,26.6375167608261)) ;
#12953 = CARTESIAN_POINT('',(52.2619374580681,40.85,26.6375167608261)) ;
#12954 = CARTESIAN_POINT('Ctrl Pts',(52.6858799643815,40.85,26.5512277126312)) ;
#12955 = CARTESIAN_POINT('Ctrl Pts',(52.4975444860756,40.85,26.6375167608261)) ;
#12956 = CARTESIAN_POINT('Ctrl Pts',(52.2619374580681,40.85,26.6375167608261)) ;
#12957 = CARTESIAN_POINT('',(52.2619374580681,41.5,26.6375167608261)) ;
#12958 = CARTESIAN_POINT('Ctrl Pts',(52.2619374580681,41.5,26.6375167608261)) ;
#12959 = CARTESIAN_POINT('Ctrl Pts',(52.2619374580681,40.85,26.6375167608261)) ;
#12960 = CARTESIAN_POINT('Ctrl Pts',(51.9633014984429,41.5,26.6375167608261)) ;
#12961 = CARTESIAN_POINT('Ctrl Pts',(51.9633014984429,40.85,26.6375167608261)) ;
#12962 = CARTESIAN_POINT('Ctrl Pts',(51.7614599056542,41.5,26.5504772901535)) ;
#12963 = CARTESIAN_POINT('Ctrl Pts',(51.7614599056542,40.85,26.5504772901535)) ;
#12964 = CARTESIAN_POINT('',(51.7614599056542,40.85,26.5504772901535)) ;
#12965 = CARTESIAN_POINT('Ctrl Pts',(52.2619374580681,40.85,26.6375167608261)) ;
#12966 = CARTESIAN_POINT('Ctrl Pts',(51.9633014984429,40.85,26.6375167608261)) ;
#12967 = CARTESIAN_POINT('Ctrl Pts',(51.7614599056542,40.85,26.5504772901535)) ;
#12968 = CARTESIAN_POINT('',(51.7614599056542,41.5,26.5504772901535)) ;
#12969 = CARTESIAN_POINT('Ctrl Pts',(51.7614599056542,41.5,26.5504772901535)) ;
#12970 = CARTESIAN_POINT('Ctrl Pts',(51.7614599056542,40.85,26.5504772901535)) ;
#12971 = CARTESIAN_POINT('Ctrl Pts',(51.5596180148423,41.5,26.4634378194809)) ;
#12972 = CARTESIAN_POINT('Ctrl Pts',(51.5596180148423,40.85,26.4634378194809)) ;
#12973 = CARTESIAN_POINT('Ctrl Pts',(51.4448158927262,41.5,26.2886081576347)) ;
#12974 = CARTESIAN_POINT('Ctrl Pts',(51.4448158927262,40.85,26.2886081576347)) ;
#12975 = CARTESIAN_POINT('',(51.4448158927262,40.85,26.2886081576347)) ;
#12976 = CARTESIAN_POINT('Ctrl Pts',(51.7614599056542,40.85,26.5504772901535)) ;
#12977 = CARTESIAN_POINT('Ctrl Pts',(51.5596180148423,40.85,26.4634378194809)) ;
#12978 = CARTESIAN_POINT('Ctrl Pts',(51.4448158927262,40.85,26.2886081576347)) ;
#12979 = CARTESIAN_POINT('',(51.4448158927262,41.5,26.2886081576347)) ;
#12980 = CARTESIAN_POINT('Ctrl Pts',(51.7787178345025,41.5,24.4375169217587)) ;
#12981 = CARTESIAN_POINT('Ctrl Pts',(51.7787178345025,40.85,24.4375169217587)) ;
#12982 = CARTESIAN_POINT('Ctrl Pts',(51.9603001065552,41.5,24.3624828696251)) ;
#12983 = CARTESIAN_POINT('Ctrl Pts',(51.9603001065552,40.85,24.3624828696251)) ;
#12984 = CARTESIAN_POINT('Ctrl Pts',(52.1824010200799,41.5,24.3624828696251)) ;
#12985 = CARTESIAN_POINT('Ctrl Pts',(52.1824010200799,40.85,24.3624828696251)) ;
#12986 = CARTESIAN_POINT('',(51.7787178345025,40.85,24.4375169217587)) ;
#12987 = CARTESIAN_POINT('',(51.7787178345025,41.5,24.4375169217587)) ;
#12988 = CARTESIAN_POINT('Ctrl Pts',(51.7787178345025,40.85,24.4375169217587)) ;
#12989 = CARTESIAN_POINT('Ctrl Pts',(51.9603001065552,40.85,24.3624828696251)) ;
#12990 = CARTESIAN_POINT('Ctrl Pts',(52.1824010200799,40.85,24.3624828696251)) ;
#12991 = CARTESIAN_POINT('Ctrl Pts',(51.5025921650231,41.5,24.6573668658733)) ;
#12992 = CARTESIAN_POINT('Ctrl Pts',(51.5025921650231,40.85,24.6573668658733)) ;
#12993 = CARTESIAN_POINT('Ctrl Pts',(51.5971352644265,41.5,24.5125509738922)) ;
#12994 = CARTESIAN_POINT('Ctrl Pts',(51.5971352644265,40.85,24.5125509738922)) ;
#12995 = CARTESIAN_POINT('Ctrl Pts',(51.7787178345025,41.5,24.4375169217587)) ;
#12996 = CARTESIAN_POINT('Ctrl Pts',(51.7787178345025,40.85,24.4375169217587)) ;
#12997 = CARTESIAN_POINT('',(51.5025921650231,40.85,24.6573668658733)) ;
#12998 = CARTESIAN_POINT('',(51.5025921650231,41.5,24.6573668658733)) ;
#12999 = CARTESIAN_POINT('Ctrl Pts',(51.5025921650231,40.85,24.6573668658733)) ;
#13000 = CARTESIAN_POINT('Ctrl Pts',(51.5971352644265,40.85,24.5125509738922)) ;
#13001 = CARTESIAN_POINT('Ctrl Pts',(51.7787178345025,40.85,24.4375169217587)) ;
#13002 = CARTESIAN_POINT('Ctrl Pts',(51.4080490656197,41.5,24.9687583684921)) ;
#13003 = CARTESIAN_POINT('Ctrl Pts',(51.4080490656197,40.85,24.9687583684921)) ;
#13004 = CARTESIAN_POINT('Ctrl Pts',(51.4080490656197,41.5,24.8021826088428)) ;
#13005 = CARTESIAN_POINT('Ctrl Pts',(51.4080490656197,40.85,24.8021826088428)) ;
#13006 = CARTESIAN_POINT('Ctrl Pts',(51.5025921650231,41.5,24.6573668658733)) ;
#13007 = CARTESIAN_POINT('Ctrl Pts',(51.5025921650231,40.85,24.6573668658733)) ;
#13008 = CARTESIAN_POINT('',(51.4080490656197,40.85,24.9687583684921)) ;
#13009 = CARTESIAN_POINT('',(51.4080490656197,41.5,24.9687583684921)) ;
#13010 = CARTESIAN_POINT('Ctrl Pts',(51.4080490656197,40.85,24.9687583684921)) ;
#13011 = CARTESIAN_POINT('Ctrl Pts',(51.4080490656197,40.85,24.8021826088428)) ;
#13012 = CARTESIAN_POINT('Ctrl Pts',(51.5025921650231,40.85,24.6573668658733)) ;
#13013 = CARTESIAN_POINT('Ctrl Pts',(51.4853342361748,41.5,25.2426329195499)) ;
#13014 = CARTESIAN_POINT('Ctrl Pts',(51.4853342361748,40.85,25.2426329195499)) ;
#13015 = CARTESIAN_POINT('Ctrl Pts',(51.4080490656197,41.5,25.1203273177147)) ;
#13016 = CARTESIAN_POINT('Ctrl Pts',(51.4080490656197,40.85,25.1203273177147)) ;
#13017 = CARTESIAN_POINT('Ctrl Pts',(51.4080490656197,41.5,24.9687583684921)) ;
#13018 = CARTESIAN_POINT('Ctrl Pts',(51.4080490656197,40.85,24.9687583684921)) ;
#13019 = CARTESIAN_POINT('',(51.4853342361748,40.85,25.2426329195499)) ;
#13020 = CARTESIAN_POINT('',(51.4853342361748,41.5,25.2426329195499)) ;
#13021 = CARTESIAN_POINT('Ctrl Pts',(51.4853342361748,40.85,25.2426329195499)) ;
#13022 = CARTESIAN_POINT('Ctrl Pts',(51.4080490656197,40.85,25.1203273177147)) ;
#13023 = CARTESIAN_POINT('Ctrl Pts',(51.4080490656197,40.85,24.9687583684921)) ;
#13024 = CARTESIAN_POINT('Ctrl Pts',(51.7201911397278,41.5,25.4474759042263)) ;
#13025 = CARTESIAN_POINT('Ctrl Pts',(51.7201911397278,40.85,25.4474759042263)) ;
#13026 = CARTESIAN_POINT('Ctrl Pts',(51.5626194067299,41.5,25.3649385213852)) ;
#13027 = CARTESIAN_POINT('Ctrl Pts',(51.5626194067299,40.85,25.3649385213852)) ;
#13028 = CARTESIAN_POINT('Ctrl Pts',(51.4853342361748,41.5,25.2426329195499)) ;
#13029 = CARTESIAN_POINT('Ctrl Pts',(51.4853342361748,40.85,25.2426329195499)) ;
#13030 = CARTESIAN_POINT('',(51.7201911397278,40.85,25.4474759042263)) ;
#13031 = CARTESIAN_POINT('',(51.7201911397278,41.5,25.4474759042263)) ;
#13032 = CARTESIAN_POINT('Ctrl Pts',(51.7201911397278,40.85,25.4474759042263)) ;
#13033 = CARTESIAN_POINT('Ctrl Pts',(51.5626194067299,40.85,25.3649385213852)) ;
#13034 = CARTESIAN_POINT('Ctrl Pts',(51.4853342361748,40.85,25.2426329195499)) ;
#13035 = CARTESIAN_POINT('Ctrl Pts',(52.1448840685189,41.5,25.5847883164883)) ;
#13036 = CARTESIAN_POINT('Ctrl Pts',(52.1448840685189,40.85,25.5847883164883)) ;
#13037 = CARTESIAN_POINT('Ctrl Pts',(51.8417461700737,41.5,25.5120052337646)) ;
#13038 = CARTESIAN_POINT('Ctrl Pts',(51.8417461700737,40.85,25.5120052337646)) ;
#13039 = CARTESIAN_POINT('Ctrl Pts',(51.7201911397278,41.5,25.4474759042263)) ;
#13040 = CARTESIAN_POINT('Ctrl Pts',(51.7201911397278,40.85,25.4474759042263)) ;
#13041 = CARTESIAN_POINT('',(52.1448840685189,40.85,25.5847883164883)) ;
#13042 = CARTESIAN_POINT('',(52.1448840685189,41.5,25.5847883164883)) ;
#13043 = CARTESIAN_POINT('Ctrl Pts',(52.1448840685189,40.85,25.5847883164883)) ;
#13044 = CARTESIAN_POINT('Ctrl Pts',(51.8417461700737,40.85,25.5120052337646)) ;
#13045 = CARTESIAN_POINT('Ctrl Pts',(51.7201911397278,40.85,25.4474759042263)) ;
#13046 = CARTESIAN_POINT('Ctrl Pts',(52.5365622825921,41.5,25.6920871078968)) ;
#13047 = CARTESIAN_POINT('Ctrl Pts',(52.5365622825921,40.85,25.6920871078968)) ;
#13048 = CARTESIAN_POINT('Ctrl Pts',(52.448021966964,41.5,25.6575713992119)) ;
#13049 = CARTESIAN_POINT('Ctrl Pts',(52.448021966964,40.85,25.6575713992119)) ;
#13050 = CARTESIAN_POINT('Ctrl Pts',(52.1448840685189,41.5,25.5847883164883)) ;
#13051 = CARTESIAN_POINT('Ctrl Pts',(52.1448840685189,40.85,25.5847883164883)) ;
#13052 = CARTESIAN_POINT('',(52.5365622825921,40.85,25.6920871078968)) ;
#13053 = CARTESIAN_POINT('',(52.5365622825921,41.5,25.6920871078968)) ;
#13054 = CARTESIAN_POINT('Ctrl Pts',(52.5365622825921,40.85,25.6920871078968)) ;
#13055 = CARTESIAN_POINT('Ctrl Pts',(52.448021966964,40.85,25.6575713992119)) ;
#13056 = CARTESIAN_POINT('Ctrl Pts',(52.1448840685189,40.85,25.5847883164883)) ;
#13057 = CARTESIAN_POINT('Ctrl Pts',(52.7346523590386,41.5,25.8218960404396)) ;
#13058 = CARTESIAN_POINT('Ctrl Pts',(52.7346523590386,40.85,25.8218960404396)) ;
#13059 = CARTESIAN_POINT('Ctrl Pts',(52.6746251173317,41.5,25.7446108698845)) ;
#13060 = CARTESIAN_POINT('Ctrl Pts',(52.6746251173317,40.85,25.7446108698845)) ;
#13061 = CARTESIAN_POINT('Ctrl Pts',(52.5365622825921,41.5,25.6920871078968)) ;
#13062 = CARTESIAN_POINT('Ctrl Pts',(52.5365622825921,40.85,25.6920871078968)) ;
#13063 = CARTESIAN_POINT('',(52.7346523590386,40.85,25.8218960404396)) ;
#13064 = CARTESIAN_POINT('',(52.7346523590386,41.5,25.8218960404396)) ;
#13065 = CARTESIAN_POINT('Ctrl Pts',(52.7346523590386,40.85,25.8218960404396)) ;
#13066 = CARTESIAN_POINT('Ctrl Pts',(52.6746251173317,40.85,25.7446108698845)) ;
#13067 = CARTESIAN_POINT('Ctrl Pts',(52.5365622825921,40.85,25.6920871078968)) ;
#13068 = CARTESIAN_POINT('Ctrl Pts',(52.7946796007454,41.5,26.0027281880379)) ;
#13069 = CARTESIAN_POINT('Ctrl Pts',(52.7946796007454,40.85,26.0027281880379)) ;
#13070 = CARTESIAN_POINT('Ctrl Pts',(52.7946796007454,41.5,25.8991812109947)) ;
#13071 = CARTESIAN_POINT('Ctrl Pts',(52.7946796007454,40.85,25.8991812109947)) ;
#13072 = CARTESIAN_POINT('Ctrl Pts',(52.7346523590386,41.5,25.8218960404396)) ;
#13073 = CARTESIAN_POINT('Ctrl Pts',(52.7346523590386,40.85,25.8218960404396)) ;
#13074 = CARTESIAN_POINT('',(52.7946796007454,40.85,26.0027281880379)) ;
#13075 = CARTESIAN_POINT('',(52.7946796007454,41.5,26.0027281880379)) ;
#13076 = CARTESIAN_POINT('Ctrl Pts',(52.7946796007454,40.85,26.0027281880379)) ;
#13077 = CARTESIAN_POINT('Ctrl Pts',(52.7946796007454,40.85,25.8991812109947)) ;
#13078 = CARTESIAN_POINT('Ctrl Pts',(52.7346523590386,40.85,25.8218960404396)) ;
#13079 = CARTESIAN_POINT('Ctrl Pts',(52.7324010916054,41.5,26.1910639643669)) ;
#13080 = CARTESIAN_POINT('Ctrl Pts',(52.7324010916054,40.85,26.1910639643669)) ;
#13081 = CARTESIAN_POINT('Ctrl Pts',(52.7946796007454,41.5,26.1047746181488)) ;
#13082 = CARTESIAN_POINT('Ctrl Pts',(52.7946796007454,40.85,26.1047746181488)) ;
#13083 = CARTESIAN_POINT('Ctrl Pts',(52.7946796007454,41.5,26.0027281880379)) ;
#13084 = CARTESIAN_POINT('Ctrl Pts',(52.7946796007454,40.85,26.0027281880379)) ;
#13085 = CARTESIAN_POINT('',(52.7324010916054,40.85,26.1910639643669)) ;
#13086 = CARTESIAN_POINT('',(52.7324010916054,41.5,26.1910639643669)) ;
#13087 = CARTESIAN_POINT('Ctrl Pts',(52.7324010916054,40.85,26.1910639643669)) ;
#13088 = CARTESIAN_POINT('Ctrl Pts',(52.7946796007454,40.85,26.1047746181488)) ;
#13089 = CARTESIAN_POINT('Ctrl Pts',(52.7946796007454,40.85,26.0027281880379)) ;
#13090 = CARTESIAN_POINT('Ctrl Pts',(52.5425647683442,41.5,26.3268758296967)) ;
#13091 = CARTESIAN_POINT('Ctrl Pts',(52.5425647683442,40.85,26.3268758296967)) ;
#13092 = CARTESIAN_POINT('Ctrl Pts',(52.6701228804886,41.5,26.277353310585)) ;
#13093 = CARTESIAN_POINT('Ctrl Pts',(52.6701228804886,40.85,26.277353310585)) ;
#13094 = CARTESIAN_POINT('Ctrl Pts',(52.7324010916054,41.5,26.1910639643669)) ;
#13095 = CARTESIAN_POINT('Ctrl Pts',(52.7324010916054,40.85,26.1910639643669)) ;
#13096 = CARTESIAN_POINT('',(52.5425647683442,40.85,26.3268758296967)) ;
#13097 = CARTESIAN_POINT('',(52.5425647683442,41.5,26.3268758296967)) ;
#13098 = CARTESIAN_POINT('Ctrl Pts',(52.5425647683442,40.85,26.3268758296967)) ;
#13099 = CARTESIAN_POINT('Ctrl Pts',(52.6701228804886,40.85,26.277353310585)) ;
#13100 = CARTESIAN_POINT('Ctrl Pts',(52.7324010916054,40.85,26.1910639643669)) ;
#13101 = CARTESIAN_POINT('Ctrl Pts',(52.248431045562,41.5,26.3763980507851)) ;
#13102 = CARTESIAN_POINT('Ctrl Pts',(52.248431045562,40.85,26.3763980507851)) ;
#13103 = CARTESIAN_POINT('Ctrl Pts',(52.4150069542229,41.5,26.3763980507851)) ;
#13104 = CARTESIAN_POINT('Ctrl Pts',(52.4150069542229,40.85,26.3763980507851)) ;
#13105 = CARTESIAN_POINT('Ctrl Pts',(52.5425647683442,41.5,26.3268758296967)) ;
#13106 = CARTESIAN_POINT('Ctrl Pts',(52.5425647683442,40.85,26.3268758296967)) ;
#13107 = CARTESIAN_POINT('',(52.248431045562,40.85,26.3763980507851)) ;
#13108 = CARTESIAN_POINT('',(52.248431045562,41.5,26.3763980507851)) ;
#13109 = CARTESIAN_POINT('Ctrl Pts',(52.248431045562,40.85,26.3763980507851)) ;
#13110 = CARTESIAN_POINT('Ctrl Pts',(52.4150069542229,40.85,26.3763980507851)) ;
#13111 = CARTESIAN_POINT('Ctrl Pts',(52.5425647683442,40.85,26.3268758296967)) ;
#13112 = CARTESIAN_POINT('Ctrl Pts',(51.9107775874436,41.5,26.3111184477806)) ;
#13113 = CARTESIAN_POINT('Ctrl Pts',(51.9107775874436,40.85,26.3111184477806)) ;
#13114 = CARTESIAN_POINT('Ctrl Pts',(52.0608459897339,41.5,26.3763980507851)) ;
#13115 = CARTESIAN_POINT('Ctrl Pts',(52.0608459897339,40.85,26.3763980507851)) ;
#13116 = CARTESIAN_POINT('Ctrl Pts',(52.248431045562,41.5,26.3763980507851)) ;
#13117 = CARTESIAN_POINT('Ctrl Pts',(52.248431045562,40.85,26.3763980507851)) ;
#13118 = CARTESIAN_POINT('',(51.9107775874436,40.85,26.3111184477806)) ;
#13119 = CARTESIAN_POINT('',(51.9107775874436,41.5,26.3111184477806)) ;
#13120 = CARTESIAN_POINT('Ctrl Pts',(51.9107775874436,40.85,26.3111184477806)) ;
#13121 = CARTESIAN_POINT('Ctrl Pts',(52.0608459897339,40.85,26.3763980507851)) ;
#13122 = CARTESIAN_POINT('Ctrl Pts',(52.248431045562,40.85,26.3763980507851)) ;
#13123 = CARTESIAN_POINT('Ctrl Pts',(51.6894270963967,41.5,26.1400408983231)) ;
#13124 = CARTESIAN_POINT('Ctrl Pts',(51.6894270963967,40.85,26.1400408983231)) ;
#13125 = CARTESIAN_POINT('Ctrl Pts',(51.7607094831765,41.5,26.2458388447762)) ;
#13126 = CARTESIAN_POINT('Ctrl Pts',(51.7607094831765,40.85,26.2458388447762)) ;
#13127 = CARTESIAN_POINT('Ctrl Pts',(51.9107775874436,41.5,26.3111184477806)) ;
#13128 = CARTESIAN_POINT('Ctrl Pts',(51.9107775874436,40.85,26.3111184477806)) ;
#13129 = CARTESIAN_POINT('',(51.6894270963967,40.85,26.1400408983231)) ;
#13130 = CARTESIAN_POINT('',(51.6894270963967,41.5,26.1400408983231)) ;
#13131 = CARTESIAN_POINT('Ctrl Pts',(51.6894270963967,40.85,26.1400408983231)) ;
#13132 = CARTESIAN_POINT('Ctrl Pts',(51.7607094831765,40.85,26.2458388447762)) ;
#13133 = CARTESIAN_POINT('Ctrl Pts',(51.9107775874436,40.85,26.3111184477806)) ;
#13134 = CARTESIAN_POINT('Ctrl Pts',(51.5986358113587,41.5,25.8691675901413)) ;
#13135 = CARTESIAN_POINT('Ctrl Pts',(51.5986358113587,40.85,25.8691675901413)) ;
#13136 = CARTESIAN_POINT('Ctrl Pts',(51.6181447096169,41.5,26.0342426538467)) ;
#13137 = CARTESIAN_POINT('Ctrl Pts',(51.6181447096169,40.85,26.0342426538467)) ;
#13138 = CARTESIAN_POINT('Ctrl Pts',(51.6894270963967,41.5,26.1400408983231)) ;
#13139 = CARTESIAN_POINT('Ctrl Pts',(51.6894270963967,40.85,26.1400408983231)) ;
#13140 = CARTESIAN_POINT('',(51.5986358113587,40.85,25.8691675901413)) ;
#13141 = CARTESIAN_POINT('',(51.5986358113587,41.5,25.8691675901413)) ;
#13142 = CARTESIAN_POINT('Ctrl Pts',(51.5986358113587,40.85,25.8691675901413)) ;
#13143 = CARTESIAN_POINT('Ctrl Pts',(51.6181447096169,40.85,26.0342426538467)) ;
#13144 = CARTESIAN_POINT('Ctrl Pts',(51.6894270963967,40.85,26.1400408983231)) ;
#13145 = CARTESIAN_POINT('Origin',(51.3240109868348,41.5,25.8931784272194)) ;
#13146 = CARTESIAN_POINT('',(51.3240109868348,40.85,25.8931784272194)) ;
#13147 = CARTESIAN_POINT('',(51.3240109868348,41.5,25.8931784272194)) ;
#13148 = CARTESIAN_POINT('',(51.3240109868348,40.85,25.8931784272194)) ;
#13149 = CARTESIAN_POINT('Ctrl Pts',(51.4448158927262,41.5,26.2886081576347)) ;
#13150 = CARTESIAN_POINT('Ctrl Pts',(51.4448158927262,40.85,26.2886081576347)) ;
#13151 = CARTESIAN_POINT('Ctrl Pts',(51.3300137706101,41.5,26.1137787938118)) ;
#13152 = CARTESIAN_POINT('Ctrl Pts',(51.3300137706101,40.85,26.1137787938118)) ;
#13153 = CARTESIAN_POINT('Ctrl Pts',(51.3240109868348,41.5,25.8931784272194)) ;
#13154 = CARTESIAN_POINT('Ctrl Pts',(51.3240109868348,40.85,25.8931784272194)) ;
#13155 = CARTESIAN_POINT('Ctrl Pts',(51.4448158927262,40.85,26.2886081576347)) ;
#13156 = CARTESIAN_POINT('Ctrl Pts',(51.3300137706101,40.85,26.1137787938118)) ;
#13157 = CARTESIAN_POINT('Ctrl Pts',(51.3240109868348,40.85,25.8931784272194)) ;
#13158 = CARTESIAN_POINT('Origin',(53.2966575417668,40.85,25.4999998152256)) ;
#13159 = CARTESIAN_POINT('Origin',(49.7077762074769,41.5,24.3999998211861)) ;
#13160 = CARTESIAN_POINT('',(49.7077762074769,40.85,24.3999998211861)) ;
#13161 = CARTESIAN_POINT('',(49.7077762074769,41.5,24.3999998211861)) ;
#13162 = CARTESIAN_POINT('',(50.0994542725384,40.85,24.3999998211861)) ;
#13163 = CARTESIAN_POINT('',(49.7077762074769,40.85,24.3999998211861)) ;
#13164 = CARTESIAN_POINT('',(50.0994542725384,41.5,24.3999998211861)) ;
#13165 = CARTESIAN_POINT('Origin',(50.0994542725384,41.5,24.3999998211861)) ;
#13166 = CARTESIAN_POINT('',(50.0994542725384,40.85,26.5999998092651)) ;
#13167 = CARTESIAN_POINT('',(50.0994542725384,40.85,24.3999998211861)) ;
#13168 = CARTESIAN_POINT('',(50.0994542725384,41.5,26.5999998092651)) ;
#13169 = CARTESIAN_POINT('Origin',(50.0994542725384,41.5,26.5999998092651)) ;
#13170 = CARTESIAN_POINT('',(49.8188268132508,40.85,26.5999998092651)) ;
#13171 = CARTESIAN_POINT('',(50.0994542725384,40.85,26.5999998092651)) ;
#13172 = CARTESIAN_POINT('',(49.8188268132508,41.5,26.5999998092651)) ;
#13173 = CARTESIAN_POINT('Origin',(49.8188268132508,41.5,26.5999998092651)) ;
#13174 = CARTESIAN_POINT('',(49.8188268132508,40.85,24.7586628735065)) ;
#13175 = CARTESIAN_POINT('',(49.8188268132508,40.85,26.5999998092651)) ;
#13176 = CARTESIAN_POINT('',(49.8188268132508,41.5,24.7586628735065)) ;
#13177 = CARTESIAN_POINT('Origin',(49.8188268132508,41.5,24.7586628735065)) ;
#13178 = CARTESIAN_POINT('',(49.179536152631,40.85,26.5999998092651)) ;
#13179 = CARTESIAN_POINT('',(49.8188268132508,40.85,24.7586628735065)) ;
#13180 = CARTESIAN_POINT('',(49.179536152631,41.5,26.5999998092651)) ;
#13181 = CARTESIAN_POINT('Origin',(49.179536152631,41.5,26.5999998092651)) ;
#13182 = CARTESIAN_POINT('',(48.916916821152,40.85,26.5999998092651)) ;
#13183 = CARTESIAN_POINT('',(49.179536152631,40.85,26.5999998092651)) ;
#13184 = CARTESIAN_POINT('',(48.916916821152,41.5,26.5999998092651)) ;
#13185 = CARTESIAN_POINT('Origin',(48.916916821152,41.5,26.5999998092651)) ;
#13186 = CARTESIAN_POINT('',(48.2806275524199,40.85,24.7271485567093)) ;
#13187 = CARTESIAN_POINT('',(48.916916821152,40.85,26.5999998092651)) ;
#13188 = CARTESIAN_POINT('',(48.2806275524199,41.5,24.7271485567093)) ;
#13189 = CARTESIAN_POINT('Origin',(48.2806275524199,41.5,24.7271485567093)) ;
#13190 = CARTESIAN_POINT('',(48.2806275524199,40.85,26.5999998092651)) ;
#13191 = CARTESIAN_POINT('',(48.2806275524199,40.85,24.7271485567093)) ;
#13192 = CARTESIAN_POINT('',(48.2806275524199,41.5,26.5999998092651)) ;
#13193 = CARTESIAN_POINT('Origin',(49.1810368485749,41.5,25.9306956768036)) ;
#13194 = CARTESIAN_POINT('',(49.1810368485749,40.85,25.9306956768036)) ;
#13195 = CARTESIAN_POINT('',(49.1810368485749,41.5,25.9306956768036)) ;
#13196 = CARTESIAN_POINT('',(49.1810368485749,40.85,25.9306956768036)) ;
#13197 = CARTESIAN_POINT('Ctrl Pts',(49.0639836080372,41.5,26.2833557963371)) ;
#13198 = CARTESIAN_POINT('Ctrl Pts',(49.0639836080372,40.85,26.2833557963371)) ;
#13199 = CARTESIAN_POINT('Ctrl Pts',(49.1015007086098,41.5,26.1633013129234)) ;
#13200 = CARTESIAN_POINT('Ctrl Pts',(49.1015007086098,40.85,26.1633013129234)) ;
#13201 = CARTESIAN_POINT('Ctrl Pts',(49.1810368485749,41.5,25.9306956768036)) ;
#13202 = CARTESIAN_POINT('Ctrl Pts',(49.1810368485749,40.85,25.9306956768036)) ;
#13203 = CARTESIAN_POINT('',(49.0639836080372,40.85,26.2833557963371)) ;
#13204 = CARTESIAN_POINT('',(49.0639836080372,41.5,26.2833557963371)) ;
#13205 = CARTESIAN_POINT('Ctrl Pts',(49.0639836080372,40.85,26.2833557963371)) ;
#13206 = CARTESIAN_POINT('Ctrl Pts',(49.1015007086098,40.85,26.1633013129234)) ;
#13207 = CARTESIAN_POINT('Ctrl Pts',(49.1810368485749,40.85,25.9306956768036)) ;
#13208 = CARTESIAN_POINT('Ctrl Pts',(48.9589358605444,41.5,25.9577079057693)) ;
#13209 = CARTESIAN_POINT('Ctrl Pts',(48.9589358605444,40.85,25.9577079057693)) ;
#13210 = CARTESIAN_POINT('Ctrl Pts',(49.0309685952961,41.5,26.1753068804741)) ;
#13211 = CARTESIAN_POINT('Ctrl Pts',(49.0309685952961,40.85,26.1753068804741)) ;
#13212 = CARTESIAN_POINT('Ctrl Pts',(49.0639836080372,41.5,26.2833557963371)) ;
#13213 = CARTESIAN_POINT('Ctrl Pts',(49.0639836080372,40.85,26.2833557963371)) ;
#13214 = CARTESIAN_POINT('',(48.9589358605444,40.85,25.9577079057693)) ;
#13215 = CARTESIAN_POINT('',(48.9589358605444,41.5,25.9577079057693)) ;
#13216 = CARTESIAN_POINT('Ctrl Pts',(48.9589358605444,40.85,25.9577079057693)) ;
#13217 = CARTESIAN_POINT('Ctrl Pts',(49.0309685952961,40.85,26.1753068804741)) ;
#13218 = CARTESIAN_POINT('Ctrl Pts',(49.0639836080372,40.85,26.2833557963371)) ;
#13219 = CARTESIAN_POINT('Origin',(48.438199210912,41.5,24.3999998211861)) ;
#13220 = CARTESIAN_POINT('',(48.438199210912,40.85,24.3999998211861)) ;
#13221 = CARTESIAN_POINT('',(48.438199210912,41.5,24.3999998211861)) ;
#13222 = CARTESIAN_POINT('',(48.438199210912,40.85,24.3999998211861)) ;
#13223 = CARTESIAN_POINT('Origin',(48.,41.5,24.3999998211861)) ;
#13224 = CARTESIAN_POINT('',(48.,40.85,24.3999998211861)) ;
#13225 = CARTESIAN_POINT('',(48.,41.5,24.3999998211861)) ;
#13226 = CARTESIAN_POINT('',(48.,40.85,24.3999998211861)) ;
#13227 = CARTESIAN_POINT('Origin',(48.,41.5,26.5999998092651)) ;
#13228 = CARTESIAN_POINT('',(48.,40.85,26.5999998092651)) ;
#13229 = CARTESIAN_POINT('',(48.,41.5,26.5999998092651)) ;
#13230 = CARTESIAN_POINT('',(48.,40.85,26.5999998092651)) ;
#13231 = CARTESIAN_POINT('Origin',(48.2806275524199,41.5,26.5999998092651)) ;
#13232 = CARTESIAN_POINT('',(48.2806275524199,40.85,26.5999998092651)) ;
#13233 = CARTESIAN_POINT('Origin',(53.2966575417668,40.85,25.4999998152256)) ;
#13234 = CARTESIAN_POINT('Origin',(45.,25.5,25.5)) ;
#13235 = CARTESIAN_POINT('',(44.25,10.4,25.5)) ;
#13236 = CARTESIAN_POINT('Origin',(44.25,25.5,25.5)) ;
#13237 = CARTESIAN_POINT('',(45.75,10.4,25.5)) ;
#13238 = CARTESIAN_POINT('',(45.,10.4,25.5)) ;
#13239 = CARTESIAN_POINT('Origin',(45.75,25.5,25.5)) ;
#13240 = CARTESIAN_POINT('Origin',(44.25,41.1,25.5)) ;
#13241 = CARTESIAN_POINT('',(44.25,10.,25.5)) ;
#13242 = CARTESIAN_POINT('Origin',(44.25,25.5,25.5)) ;
#13243 = CARTESIAN_POINT('Origin',(45.75,40.6,25.5)) ;
#13244 = CARTESIAN_POINT('Origin',(55.25,25.5,25.5)) ;
#13245 = CARTESIAN_POINT('Origin',(33.85,11.357864376269,39.642135623731)) ;
#13246 = CARTESIAN_POINT('',(34.,13.4700501879138,35.8966488600263)) ;
#13247 = CARTESIAN_POINT('',(33.7,13.3226883871013,36.1579618900522)) ;
#13248 = CARTESIAN_POINT('',(34.,13.4700501879138,35.8966488600263)) ;
#13249 = CARTESIAN_POINT('',(33.7,11.357864376269,43.642135623731)) ;
#13250 = CARTESIAN_POINT('Origin',(33.7,11.357864376269,39.642135623731)) ;
#13251 = CARTESIAN_POINT('',(33.7,14.8420381099478,37.6773116128987)) ;
#13252 = CARTESIAN_POINT('Origin',(33.7,11.357864376269,39.642135623731)) ;
#13253 = CARTESIAN_POINT('',(34.,15.1033511399737,37.5299498120862)) ;
#13254 = CARTESIAN_POINT('',(33.7,14.8420381099478,37.6773116128987)) ;
#13255 = CARTESIAN_POINT('Origin',(34.,11.357864376269,39.642135623731)) ;
#13256 = CARTESIAN_POINT('Ctrl Pts',(34.,15.1033511399737,37.5299498120862)) ;
#13257 = CARTESIAN_POINT('Ctrl Pts',(34.,14.9939502140824,37.3359518609572)) ;
#13258 = CARTESIAN_POINT('Ctrl Pts',(34.0395441492995,14.7425871058727,36.9664669273901)) ;
#13259 = CARTESIAN_POINT('Ctrl Pts',(34.0658646655374,14.2092063101249,36.3963307672773)) ;
#13260 = CARTESIAN_POINT('Ctrl Pts',(34.,13.7610471146074,36.0607502488633)) ;
#13261 = CARTESIAN_POINT('Ctrl Pts',(34.,13.4700501879138,35.8966488600263)) ;
#13262 = CARTESIAN_POINT('Ctrl Pts',(33.9,15.0162467966317,37.579070412357)) ;
#13263 = CARTESIAN_POINT('Ctrl Pts',(33.9,14.9093900783193,37.3895840414868)) ;
#13264 = CARTESIAN_POINT('Ctrl Pts',(33.9263627661997,14.66459918252,37.0282402745978)) ;
#13265 = CARTESIAN_POINT('Ctrl Pts',(33.9439097770249,14.1443737517734,36.4701794174857)) ;
#13266 = CARTESIAN_POINT('Ctrl Pts',(33.9,13.7051591439483,36.1440382808369)) ;
#13267 = CARTESIAN_POINT('Ctrl Pts',(33.9,13.4209295876429,35.9837532033683)) ;
#13268 = CARTESIAN_POINT('Ctrl Pts',(33.8,14.9291424532898,37.6281910126279)) ;
#13269 = CARTESIAN_POINT('Ctrl Pts',(33.8,14.8248299425562,37.4432162220164)) ;
#13270 = CARTESIAN_POINT('Ctrl Pts',(33.8131813830998,14.5866112591672,37.0900136218054)) ;
#13271 = CARTESIAN_POINT('Ctrl Pts',(33.8219548885125,14.0795411934218,36.5440280676941)) ;
#13272 = CARTESIAN_POINT('Ctrl Pts',(33.8,13.6492711732893,36.2273263128106)) ;
#13273 = CARTESIAN_POINT('Ctrl Pts',(33.8,13.3718089873721,36.0708575467102)) ;
#13274 = CARTESIAN_POINT('Ctrl Pts',(33.7,14.8420381099478,37.6773116128987)) ;
#13275 = CARTESIAN_POINT('Ctrl Pts',(33.7,14.7402698067931,37.496848402546)) ;
#13276 = CARTESIAN_POINT('Ctrl Pts',(33.7,14.5086233358145,37.151786969013)) ;
#13277 = CARTESIAN_POINT('Ctrl Pts',(33.7,14.0147086350703,36.6178767179025)) ;
#13278 = CARTESIAN_POINT('Ctrl Pts',(33.7,13.5933832026303,36.3106143447843)) ;
#13279 = CARTESIAN_POINT('Ctrl Pts',(33.7,13.3226883871013,36.1579618900522)) ;
#13280 = CARTESIAN_POINT('Ctrl Pts',(34.,13.4700501879138,35.8966488600263)) ;
#13281 = CARTESIAN_POINT('Ctrl Pts',(34.,13.7610471146074,36.0607502488633)) ;
#13282 = CARTESIAN_POINT('Ctrl Pts',(34.0658646655374,14.2092063101249,36.3963307672773)) ;
#13283 = CARTESIAN_POINT('Ctrl Pts',(34.0395441492995,14.7425871058727,36.9664669273901)) ;
#13284 = CARTESIAN_POINT('Ctrl Pts',(34.,14.9939502140824,37.3359518609572)) ;
#13285 = CARTESIAN_POINT('Ctrl Pts',(34.,15.1033511399737,37.5299498120862)) ;
#13286 = CARTESIAN_POINT('Ctrl Pts',(33.7,14.8420381099478,37.6773116128987)) ;
#13287 = CARTESIAN_POINT('Ctrl Pts',(33.7,14.7402698067931,37.496848402546)) ;
#13288 = CARTESIAN_POINT('Ctrl Pts',(33.7,14.5086233358145,37.151786969013)) ;
#13289 = CARTESIAN_POINT('Ctrl Pts',(33.7,14.0147086350703,36.6178767179025)) ;
#13290 = CARTESIAN_POINT('Ctrl Pts',(33.7,13.5933832026303,36.3106143447843)) ;
#13291 = CARTESIAN_POINT('Ctrl Pts',(33.7,13.3226883871013,36.1579618900522)) ;
#13292 = CARTESIAN_POINT('Origin',(34.4,25.5,25.5)) ;
#13293 = CARTESIAN_POINT('',(34.,13.4700501879138,15.1033511399737)) ;
#13294 = CARTESIAN_POINT('Origin',(34.,25.5,25.5)) ;
#13295 = CARTESIAN_POINT('',(34.,15.1033511399737,13.4700501879138)) ;
#13296 = CARTESIAN_POINT('Ctrl Pts',(34.,15.1033511399737,13.4700501879138)) ;
#13297 = CARTESIAN_POINT('Ctrl Pts',(34.,14.9939502140824,13.6640481390428)) ;
#13298 = CARTESIAN_POINT('Ctrl Pts',(34.0395562744413,14.7425990198672,14.0335422105128)) ;
#13299 = CARTESIAN_POINT('Ctrl Pts',(34.0658862423307,14.2092225347123,14.6036824431284)) ;
#13300 = CARTESIAN_POINT('Ctrl Pts',(34.,13.7610471146074,14.9392497511367)) ;
#13301 = CARTESIAN_POINT('Ctrl Pts',(34.,13.4700501879138,15.1033511399737)) ;
#13302 = CARTESIAN_POINT('',(34.,35.8966488600263,13.4700501879138)) ;
#13303 = CARTESIAN_POINT('Origin',(34.,25.5,25.5)) ;
#13304 = CARTESIAN_POINT('',(34.,37.5299498120862,15.1033511399737)) ;
#13305 = CARTESIAN_POINT('Ctrl Pts',(34.,37.5299498120862,15.1033511399737)) ;
#13306 = CARTESIAN_POINT('Ctrl Pts',(34.,37.2389528853926,14.9392497511367)) ;
#13307 = CARTESIAN_POINT('Ctrl Pts',(34.0658646655374,36.790793689875,14.6036692327227)) ;
#13308 = CARTESIAN_POINT('Ctrl Pts',(34.0395441492995,36.2574128941273,14.0335330726099)) ;
#13309 = CARTESIAN_POINT('Ctrl Pts',(34.,36.0060497859176,13.6640481390428)) ;
#13310 = CARTESIAN_POINT('Ctrl Pts',(34.,35.8966488600263,13.4700501879138)) ;
#13311 = CARTESIAN_POINT('',(34.,37.5299498120862,35.8966488600263)) ;
#13312 = CARTESIAN_POINT('Origin',(34.,25.5,25.5)) ;
#13313 = CARTESIAN_POINT('',(34.,35.8966488600263,37.5299498120862)) ;
#13314 = CARTESIAN_POINT('Ctrl Pts',(34.,35.8966488600263,37.5299498120862)) ;
#13315 = CARTESIAN_POINT('Ctrl Pts',(34.,36.0060497859176,37.3359518609572)) ;
#13316 = CARTESIAN_POINT('Ctrl Pts',(34.0395377031192,36.2574192030825,36.9664717701347)) ;
#13317 = CARTESIAN_POINT('Ctrl Pts',(34.0658532948882,36.7908022610815,36.3963377418929)) ;
#13318 = CARTESIAN_POINT('Ctrl Pts',(34.,37.2389528853926,36.0607502488633)) ;
#13319 = CARTESIAN_POINT('Ctrl Pts',(34.,37.5299498120862,35.8966488600263)) ;
#13320 = CARTESIAN_POINT('',(34.,25.5,41.4)) ;
#13321 = CARTESIAN_POINT('Origin',(34.,25.5,25.5)) ;
#13322 = CARTESIAN_POINT('',(34.4,25.5,41.)) ;
#13323 = CARTESIAN_POINT('Origin',(34.4,25.5,41.4)) ;
#13324 = CARTESIAN_POINT('',(34.4,10.,25.5)) ;
#13325 = CARTESIAN_POINT('Origin',(34.4,25.5,25.5)) ;
#13326 = CARTESIAN_POINT('Origin',(34.4,25.5,25.5)) ;
#13327 = CARTESIAN_POINT('Origin',(34.,25.5,25.5)) ;
#13328 = CARTESIAN_POINT('Origin',(34.,11.357864376269,39.642135623731)) ;
#13329 = CARTESIAN_POINT('',(29.6,11.357864376269,43.642135623731)) ;
#13330 = CARTESIAN_POINT('',(34.,11.357864376269,43.642135623731)) ;
#13331 = CARTESIAN_POINT('Origin',(29.6,11.357864376269,39.642135623731)) ;
#13332 = CARTESIAN_POINT('Origin',(33.85,39.642135623731,39.642135623731)) ;
#13333 = CARTESIAN_POINT('',(33.7,36.1579618900522,37.6773116128987)) ;
#13334 = CARTESIAN_POINT('',(34.,35.8966488600263,37.5299498120862)) ;
#13335 = CARTESIAN_POINT('',(33.7,39.642135623731,43.642135623731)) ;
#13336 = CARTESIAN_POINT('Origin',(33.7,39.642135623731,39.642135623731)) ;
#13337 = CARTESIAN_POINT('',(33.7,37.6773116128987,36.1579618900522)) ;
#13338 = CARTESIAN_POINT('Origin',(33.7,39.642135623731,39.642135623731)) ;
#13339 = CARTESIAN_POINT('',(33.7,37.6773116128987,36.1579618900522)) ;
#13340 = CARTESIAN_POINT('Origin',(34.,39.642135623731,39.642135623731)) ;
#13341 = CARTESIAN_POINT('Ctrl Pts',(34.,37.5299498120862,35.8966488600263)) ;
#13342 = CARTESIAN_POINT('Ctrl Pts',(34.,37.2389528853926,36.0607502488633)) ;
#13343 = CARTESIAN_POINT('Ctrl Pts',(34.0658532948882,36.7908022610815,36.3963377418929)) ;
#13344 = CARTESIAN_POINT('Ctrl Pts',(34.0395377031192,36.2574192030825,36.9664717701347)) ;
#13345 = CARTESIAN_POINT('Ctrl Pts',(34.,36.0060497859176,37.3359518609572)) ;
#13346 = CARTESIAN_POINT('Ctrl Pts',(34.,35.8966488600263,37.5299498120862)) ;
#13347 = CARTESIAN_POINT('Ctrl Pts',(33.9,37.579070412357,35.9837532033683)) ;
#13348 = CARTESIAN_POINT('Ctrl Pts',(33.9,37.2948408560517,36.1440382808369)) ;
#13349 = CARTESIAN_POINT('Ctrl Pts',(33.9439021965921,36.8556320186083,36.4701841374116)) ;
#13350 = CARTESIAN_POINT('Ctrl Pts',(33.9263584687462,36.3354050597151,37.0282435448734)) ;
#13351 = CARTESIAN_POINT('Ctrl Pts',(33.9,36.0906099216807,37.3895840414868)) ;
#13352 = CARTESIAN_POINT('Ctrl Pts',(33.9,35.9837532033683,37.579070412357)) ;
#13353 = CARTESIAN_POINT('Ctrl Pts',(33.8,37.6281910126279,36.0708575467102)) ;
#13354 = CARTESIAN_POINT('Ctrl Pts',(33.8,37.3507288267107,36.2273263128106)) ;
#13355 = CARTESIAN_POINT('Ctrl Pts',(33.8219510982961,36.9204617761351,36.5440305329303)) ;
#13356 = CARTESIAN_POINT('Ctrl Pts',(33.8131792343731,36.4133909163477,37.090015319612)) ;
#13357 = CARTESIAN_POINT('Ctrl Pts',(33.8,36.1751700574438,37.4432162220164)) ;
#13358 = CARTESIAN_POINT('Ctrl Pts',(33.8,36.0708575467102,37.6281910126279)) ;
#13359 = CARTESIAN_POINT('Ctrl Pts',(33.7,37.6773116128987,36.1579618900522)) ;
#13360 = CARTESIAN_POINT('Ctrl Pts',(33.7,37.4066167973697,36.3106143447843)) ;
#13361 = CARTESIAN_POINT('Ctrl Pts',(33.7,36.9852915336619,36.6178769284489)) ;
#13362 = CARTESIAN_POINT('Ctrl Pts',(33.7,36.4913767729803,37.1517870943507)) ;
#13363 = CARTESIAN_POINT('Ctrl Pts',(33.7,36.2597301932069,37.496848402546)) ;
#13364 = CARTESIAN_POINT('Ctrl Pts',(33.7,36.1579618900522,37.6773116128987)) ;
#13365 = CARTESIAN_POINT('Ctrl Pts',(33.7,37.6773116128987,36.1579618900522)) ;
#13366 = CARTESIAN_POINT('Ctrl Pts',(33.7,37.4066167973697,36.3106143447843)) ;
#13367 = CARTESIAN_POINT('Ctrl Pts',(33.7,36.9852915336619,36.6178769284489)) ;
#13368 = CARTESIAN_POINT('Ctrl Pts',(33.7,36.4913767729803,37.1517870943507)) ;
#13369 = CARTESIAN_POINT('Ctrl Pts',(33.7,36.2597301932069,37.496848402546)) ;
#13370 = CARTESIAN_POINT('Ctrl Pts',(33.7,36.1579618900522,37.6773116128987)) ;
#13371 = CARTESIAN_POINT('Origin',(34.,39.642135623731,39.642135623731)) ;
#13372 = CARTESIAN_POINT('',(29.6,39.642135623731,43.642135623731)) ;
#13373 = CARTESIAN_POINT('',(34.,39.642135623731,43.642135623731)) ;
#13374 = CARTESIAN_POINT('Origin',(29.6,39.642135623731,39.642135623731)) ;
#13375 = CARTESIAN_POINT('Origin',(33.85,39.642135623731,11.3578643762691)) ;
#13376 = CARTESIAN_POINT('',(33.7,37.6773116128987,14.8420381099478)) ;
#13377 = CARTESIAN_POINT('',(34.,37.5299498120862,15.1033511399737)) ;
#13378 = CARTESIAN_POINT('',(33.7,39.642135623731,15.3578643762691)) ;
#13379 = CARTESIAN_POINT('Origin',(33.7,39.642135623731,11.3578643762691)) ;
#13380 = CARTESIAN_POINT('',(33.7,36.1579618900522,13.3226883871013)) ;
#13381 = CARTESIAN_POINT('Origin',(33.7,39.642135623731,11.3578643762691)) ;
#13382 = CARTESIAN_POINT('',(33.7,36.1579618900522,13.3226883871013)) ;
#13383 = CARTESIAN_POINT('Origin',(34.,39.642135623731,11.3578643762691)) ;
#13384 = CARTESIAN_POINT('Ctrl Pts',(34.,35.8966488600263,13.4700501879138)) ;
#13385 = CARTESIAN_POINT('Ctrl Pts',(34.,36.0060497859176,13.6640481390428)) ;
#13386 = CARTESIAN_POINT('Ctrl Pts',(34.0395441492995,36.2574128941273,14.0335330726099)) ;
#13387 = CARTESIAN_POINT('Ctrl Pts',(34.0658646655374,36.790793689875,14.6036692327227)) ;
#13388 = CARTESIAN_POINT('Ctrl Pts',(34.,37.2389528853926,14.9392497511367)) ;
#13389 = CARTESIAN_POINT('Ctrl Pts',(34.,37.5299498120862,15.1033511399737)) ;
#13390 = CARTESIAN_POINT('Ctrl Pts',(33.9,35.9837532033683,13.420929587643)) ;
#13391 = CARTESIAN_POINT('Ctrl Pts',(33.9,36.0906099216807,13.6104159585132)) ;
#13392 = CARTESIAN_POINT('Ctrl Pts',(33.9263627661997,36.33540081748,13.9717597254023)) ;
#13393 = CARTESIAN_POINT('Ctrl Pts',(33.9439097770249,36.8556262482266,14.5298205825143)) ;
#13394 = CARTESIAN_POINT('Ctrl Pts',(33.9,37.2948408560517,14.8559617191631)) ;
#13395 = CARTESIAN_POINT('Ctrl Pts',(33.9,37.579070412357,15.0162467966317)) ;
#13396 = CARTESIAN_POINT('Ctrl Pts',(33.8,36.0708575467102,13.3718089873721)) ;
#13397 = CARTESIAN_POINT('Ctrl Pts',(33.8,36.1751700574438,13.5567837779836)) ;
#13398 = CARTESIAN_POINT('Ctrl Pts',(33.8131813830998,36.4133887408328,13.9099863781946)) ;
#13399 = CARTESIAN_POINT('Ctrl Pts',(33.8219548885125,36.9204588065782,14.4559719323059)) ;
#13400 = CARTESIAN_POINT('Ctrl Pts',(33.8,37.3507288267107,14.7726736871894)) ;
#13401 = CARTESIAN_POINT('Ctrl Pts',(33.8,37.6281910126279,14.9291424532898)) ;
#13402 = CARTESIAN_POINT('Ctrl Pts',(33.7,36.1579618900522,13.3226883871013)) ;
#13403 = CARTESIAN_POINT('Ctrl Pts',(33.7,36.2597301932069,13.503151597454)) ;
#13404 = CARTESIAN_POINT('Ctrl Pts',(33.7,36.4913766641855,13.848213030987)) ;
#13405 = CARTESIAN_POINT('Ctrl Pts',(33.7,36.9852913649297,14.3821232820975)) ;
#13406 = CARTESIAN_POINT('Ctrl Pts',(33.7,37.4066167973697,14.6893856552157)) ;
#13407 = CARTESIAN_POINT('Ctrl Pts',(33.7,37.6773116128987,14.8420381099478)) ;
#13408 = CARTESIAN_POINT('Ctrl Pts',(33.7,36.1579618900522,13.3226883871013)) ;
#13409 = CARTESIAN_POINT('Ctrl Pts',(33.7,36.2597301932069,13.503151597454)) ;
#13410 = CARTESIAN_POINT('Ctrl Pts',(33.7,36.4913766641855,13.848213030987)) ;
#13411 = CARTESIAN_POINT('Ctrl Pts',(33.7,36.9852913649297,14.3821232820975)) ;
#13412 = CARTESIAN_POINT('Ctrl Pts',(33.7,37.4066167973697,14.6893856552157)) ;
#13413 = CARTESIAN_POINT('Ctrl Pts',(33.7,37.6773116128987,14.8420381099478)) ;
#13414 = CARTESIAN_POINT('Origin',(34.,39.642135623731,11.3578643762691)) ;
#13415 = CARTESIAN_POINT('',(29.6,39.642135623731,15.3578643762691)) ;
#13416 = CARTESIAN_POINT('',(34.,39.642135623731,15.3578643762691)) ;
#13417 = CARTESIAN_POINT('Origin',(29.6,39.642135623731,11.3578643762691)) ;
#13418 = CARTESIAN_POINT('Origin',(33.85,11.3578643762691,11.357864376269)) ;
#13419 = CARTESIAN_POINT('',(33.7,14.8420381099478,13.3226883871013)) ;
#13420 = CARTESIAN_POINT('',(34.,15.1033511399737,13.4700501879138)) ;
#13421 = CARTESIAN_POINT('',(33.7,11.3578643762691,15.357864376269)) ;
#13422 = CARTESIAN_POINT('Origin',(33.7,11.3578643762691,11.357864376269)) ;
#13423 = CARTESIAN_POINT('',(33.7,13.3226883871013,14.8420381099478)) ;
#13424 = CARTESIAN_POINT('Origin',(33.7,11.3578643762691,11.357864376269)) ;
#13425 = CARTESIAN_POINT('',(33.7,13.3226883871013,14.8420381099478)) ;
#13426 = CARTESIAN_POINT('Origin',(34.,11.3578643762691,11.357864376269)) ;
#13427 = CARTESIAN_POINT('Ctrl Pts',(34.,13.4700501879138,15.1033511399737)) ;
#13428 = CARTESIAN_POINT('Ctrl Pts',(34.,13.7610471146074,14.9392497511367)) ;
#13429 = CARTESIAN_POINT('Ctrl Pts',(34.0658862423307,14.2092225347123,14.6036824431284)) ;
#13430 = CARTESIAN_POINT('Ctrl Pts',(34.0395562744413,14.7425990198672,14.0335422105128)) ;
#13431 = CARTESIAN_POINT('Ctrl Pts',(34.,14.9939502140824,13.6640481390428)) ;
#13432 = CARTESIAN_POINT('Ctrl Pts',(34.,15.1033511399737,13.4700501879138)) ;
#13433 = CARTESIAN_POINT('Ctrl Pts',(33.9,13.420929587643,15.0162467966317)) ;
#13434 = CARTESIAN_POINT('Ctrl Pts',(33.9,13.7051591439483,14.8559617191631)) ;
#13435 = CARTESIAN_POINT('Ctrl Pts',(33.9439241615538,14.1443846747721,14.5298295225732)) ;
#13436 = CARTESIAN_POINT('Ctrl Pts',(33.9263708496276,14.6646071935385,13.971765895988)) ;
#13437 = CARTESIAN_POINT('Ctrl Pts',(33.9,14.9093900783193,13.6104159585132)) ;
#13438 = CARTESIAN_POINT('Ctrl Pts',(33.9,15.0162467966317,13.4209295876429)) ;
#13439 = CARTESIAN_POINT('Ctrl Pts',(33.8,13.3718089873721,14.9291424532898)) ;
#13440 = CARTESIAN_POINT('Ctrl Pts',(33.8,13.6492711732893,14.7726736871894)) ;
#13441 = CARTESIAN_POINT('Ctrl Pts',(33.8219620807769,14.0795468148318,14.455976602018)) ;
#13442 = CARTESIAN_POINT('Ctrl Pts',(33.8131854248138,14.5866153672098,13.9099895814631)) ;
#13443 = CARTESIAN_POINT('Ctrl Pts',(33.8,14.8248299425562,13.5567837779836)) ;
#13444 = CARTESIAN_POINT('Ctrl Pts',(33.8,14.9291424532898,13.3718089873721)) ;
#13445 = CARTESIAN_POINT('Ctrl Pts',(33.7,13.3226883871013,14.8420381099478)) ;
#13446 = CARTESIAN_POINT('Ctrl Pts',(33.7,13.5933832026303,14.6893856552157)) ;
#13447 = CARTESIAN_POINT('Ctrl Pts',(33.7,14.0147089548915,14.3821236814628)) ;
#13448 = CARTESIAN_POINT('Ctrl Pts',(33.7,14.5086235408811,13.8482132669383)) ;
#13449 = CARTESIAN_POINT('Ctrl Pts',(33.7,14.7402698067931,13.503151597454)) ;
#13450 = CARTESIAN_POINT('Ctrl Pts',(33.7,14.8420381099478,13.3226883871013)) ;
#13451 = CARTESIAN_POINT('Ctrl Pts',(33.7,13.3226883871013,14.8420381099478)) ;
#13452 = CARTESIAN_POINT('Ctrl Pts',(33.7,13.5933832026303,14.6893856552157)) ;
#13453 = CARTESIAN_POINT('Ctrl Pts',(33.7,14.0147089548915,14.3821236814628)) ;
#13454 = CARTESIAN_POINT('Ctrl Pts',(33.7,14.5086235408811,13.8482132669383)) ;
#13455 = CARTESIAN_POINT('Ctrl Pts',(33.7,14.7402698067931,13.503151597454)) ;
#13456 = CARTESIAN_POINT('Ctrl Pts',(33.7,14.8420381099478,13.3226883871013)) ;
#13457 = CARTESIAN_POINT('Origin',(34.,11.3578643762691,11.357864376269)) ;
#13458 = CARTESIAN_POINT('',(29.6,11.3578643762691,15.357864376269)) ;
#13459 = CARTESIAN_POINT('',(34.,11.3578643762691,15.357864376269)) ;
#13460 = CARTESIAN_POINT('Origin',(29.6,11.3578643762691,11.357864376269)) ;
#13461 = CARTESIAN_POINT('Origin',(29.6,11.3578643762691,11.357864376269)) ;
#13462 = CARTESIAN_POINT('',(29.6,11.3578643762691,13.607864376269)) ;
#13463 = CARTESIAN_POINT('Origin',(29.6,11.3578643762691,11.357864376269)) ;
#13464 = CARTESIAN_POINT('Origin',(29.6,39.642135623731,11.3578643762691)) ;
#13465 = CARTESIAN_POINT('',(29.6,39.642135623731,13.607864376269)) ;
#13466 = CARTESIAN_POINT('Origin',(29.6,39.642135623731,11.3578643762691)) ;
#13467 = CARTESIAN_POINT('Origin',(29.6,39.642135623731,39.642135623731)) ;
#13468 = CARTESIAN_POINT('',(29.6,39.642135623731,41.892135623731)) ;
#13469 = CARTESIAN_POINT('Origin',(29.6,39.642135623731,39.642135623731)) ;
#13470 = CARTESIAN_POINT('Origin',(29.6,11.357864376269,39.642135623731)) ;
#13471 = CARTESIAN_POINT('',(29.6,11.357864376269,41.892135623731)) ;
#13472 = CARTESIAN_POINT('Origin',(29.6,11.357864376269,39.642135623731)) ;
#13473 = CARTESIAN_POINT('Origin',(34.,11.3578643762691,11.357864376269)) ;
#13474 = CARTESIAN_POINT('',(27.,11.3578643762691,13.607864376269)) ;
#13475 = CARTESIAN_POINT('',(34.,11.3578643762691,13.607864376269)) ;
#13476 = CARTESIAN_POINT('Origin',(27.,11.3578643762691,11.357864376269)) ;
#13477 = CARTESIAN_POINT('Origin',(34.,39.642135623731,11.3578643762691)) ;
#13478 = CARTESIAN_POINT('',(27.,39.642135623731,13.607864376269)) ;
#13479 = CARTESIAN_POINT('',(34.,39.642135623731,13.607864376269)) ;
#13480 = CARTESIAN_POINT('Origin',(27.,39.642135623731,11.3578643762691)) ;
#13481 = CARTESIAN_POINT('Origin',(34.,39.642135623731,39.642135623731)) ;
#13482 = CARTESIAN_POINT('',(27.,39.642135623731,41.892135623731)) ;
#13483 = CARTESIAN_POINT('',(34.,39.642135623731,41.892135623731)) ;
#13484 = CARTESIAN_POINT('Origin',(27.,39.642135623731,39.642135623731)) ;
#13485 = CARTESIAN_POINT('Origin',(34.,11.357864376269,39.642135623731)) ;
#13486 = CARTESIAN_POINT('',(27.,11.357864376269,41.892135623731)) ;
#13487 = CARTESIAN_POINT('',(34.,11.357864376269,41.892135623731)) ;
#13488 = CARTESIAN_POINT('Origin',(27.,11.357864376269,39.642135623731)) ;
#13489 = CARTESIAN_POINT('Origin',(32.1,19.8431457505076,19.8431457505076)) ;
#13490 = CARTESIAN_POINT('',(32.1,20.6453165160457,18.4012643188649)) ;
#13491 = CARTESIAN_POINT('',(71.9,20.6453165160457,18.4012643188649)) ;
#13492 = CARTESIAN_POINT('',(32.1,20.6453165160457,18.4012643188649)) ;
#13493 = CARTESIAN_POINT('',(32.1,18.4012643188649,20.6453165160456)) ;
#13494 = CARTESIAN_POINT('Origin',(32.1,19.8431457505076,19.8431457505076)) ;
#13495 = CARTESIAN_POINT('',(71.9,18.4012643188649,20.6453165160456)) ;
#13496 = CARTESIAN_POINT('',(32.1,18.4012643188649,20.6453165160456)) ;
#13497 = CARTESIAN_POINT('Origin',(71.9,19.8431457505076,19.8431457505076)) ;
#13498 = CARTESIAN_POINT('Origin',(32.1,31.1568542494924,19.8431457505076)) ;
#13499 = CARTESIAN_POINT('',(32.1,32.5987356811351,20.6453165160457)) ;
#13500 = CARTESIAN_POINT('',(71.9,32.5987356811351,20.6453165160457)) ;
#13501 = CARTESIAN_POINT('',(32.1,32.5987356811351,20.6453165160457)) ;
#13502 = CARTESIAN_POINT('',(32.1,30.3546834839544,18.4012643188649)) ;
#13503 = CARTESIAN_POINT('Origin',(32.1,31.1568542494924,19.8431457505076)) ;
#13504 = CARTESIAN_POINT('',(71.9,30.3546834839544,18.4012643188649)) ;
#13505 = CARTESIAN_POINT('',(32.1,30.3546834839544,18.4012643188649)) ;
#13506 = CARTESIAN_POINT('Origin',(71.9,31.1568542494924,19.8431457505076)) ;
#13507 = CARTESIAN_POINT('Origin',(32.1,31.1568542494924,31.1568542494924)) ;
#13508 = CARTESIAN_POINT('',(71.9,32.5987356811351,30.3546834839544)) ;
#13509 = CARTESIAN_POINT('',(32.1,32.5987356811351,30.3546834839544)) ;
#13510 = CARTESIAN_POINT('',(32.1,32.5987356811351,30.3546834839544)) ;
#13511 = CARTESIAN_POINT('',(71.9,30.3546834839544,32.5987356811351)) ;
#13512 = CARTESIAN_POINT('Origin',(71.9,31.1568542494924,31.1568542494924)) ;
#13513 = CARTESIAN_POINT('',(32.1,30.3546834839544,32.5987356811351)) ;
#13514 = CARTESIAN_POINT('',(32.1,30.3546834839544,32.5987356811351)) ;
#13515 = CARTESIAN_POINT('Origin',(32.1,31.1568542494924,31.1568542494924)) ;
#13516 = CARTESIAN_POINT('Origin',(32.1,19.8431457505076,31.1568542494924)) ;
#13517 = CARTESIAN_POINT('',(71.9,20.6453165160456,32.5987356811351)) ;
#13518 = CARTESIAN_POINT('',(32.1,20.6453165160456,32.5987356811351)) ;
#13519 = CARTESIAN_POINT('',(32.1,20.6453165160456,32.5987356811351)) ;
#13520 = CARTESIAN_POINT('',(71.9,18.4012643188649,30.3546834839544)) ;
#13521 = CARTESIAN_POINT('Origin',(71.9,19.8431457505076,31.1568542494924)) ;
#13522 = CARTESIAN_POINT('',(32.1,18.4012643188649,30.3546834839544)) ;
#13523 = CARTESIAN_POINT('',(32.1,18.4012643188649,30.3546834839544)) ;
#13524 = CARTESIAN_POINT('Origin',(32.1,19.8431457505076,31.1568542494924)) ;
#13525 = CARTESIAN_POINT('Origin',(71.9,34.1,25.5)) ;
#13526 = CARTESIAN_POINT('',(71.9,13.5,25.5)) ;
#13527 = CARTESIAN_POINT('Origin',(71.9,25.5,25.5)) ;
#13528 = CARTESIAN_POINT('Origin',(71.9,25.5,25.5)) ;
#13529 = CARTESIAN_POINT('Origin',(71.9,25.5,25.5)) ;
#13530 = CARTESIAN_POINT('Origin',(71.9,25.5,25.5)) ;
#13531 = CARTESIAN_POINT('Origin',(71.9,25.5,25.5)) ;
#13532 = CARTESIAN_POINT('Origin',(52.,25.5,25.5)) ;
#13533 = CARTESIAN_POINT('Origin',(32.1,25.5,25.5)) ;
#13534 = CARTESIAN_POINT('Origin',(52.,25.5,25.5)) ;
#13535 = CARTESIAN_POINT('Origin',(32.1,25.5,25.5)) ;
#13536 = CARTESIAN_POINT('Origin',(52.,25.5,25.5)) ;
#13537 = CARTESIAN_POINT('Origin',(32.1,25.5,25.5)) ;
#13538 = CARTESIAN_POINT('Origin',(52.,25.5,25.5)) ;
#13539 = CARTESIAN_POINT('Origin',(32.1,25.5,25.5)) ;
#13540 = CARTESIAN_POINT('Origin',(34.,41.,25.5)) ;
#13541 = CARTESIAN_POINT('',(34.,0.500000000000001,25.5)) ;
#13542 = CARTESIAN_POINT('Origin',(34.,25.5,25.5)) ;
#13543 = CARTESIAN_POINT('Origin',(55.25,25.5,25.5)) ;
#13544 = CARTESIAN_POINT('',(55.25,10.,25.5)) ;
#13545 = CARTESIAN_POINT('Origin',(74.9,38.1,25.5)) ;
#13546 = CARTESIAN_POINT('',(74.9,12.9,25.5)) ;
#13547 = CARTESIAN_POINT('Origin',(74.9,25.5,25.5)) ;
#13548 = CARTESIAN_POINT('',(74.9,13.5,25.5)) ;
#13549 = CARTESIAN_POINT('Origin',(74.9,25.5,25.5)) ;
#13550 = CARTESIAN_POINT('Origin',(75.55,25.5,25.5)) ;
#13551 = CARTESIAN_POINT('',(76.2,12.9,25.5)) ;
#13552 = CARTESIAN_POINT('',(75.55,12.9,25.5)) ;
#13553 = CARTESIAN_POINT('Origin',(76.2,25.5,25.5)) ;
#13554 = CARTESIAN_POINT('Origin',(76.2,37.4,25.5)) ;
#13555 = CARTESIAN_POINT('',(76.2,13.5,25.5)) ;
#13556 = CARTESIAN_POINT('Origin',(76.2,25.5,25.5)) ;
#13557 = CARTESIAN_POINT('Origin',(74.45,25.5,25.5)) ;
#13558 = CARTESIAN_POINT('',(77.,13.5,25.5)) ;
#13559 = CARTESIAN_POINT('Origin',(77.,25.5,25.5)) ;
#13560 = CARTESIAN_POINT('',(74.45,13.5,25.5)) ;
#13561 = CARTESIAN_POINT('Origin',(27.8,38.1,25.5)) ;
#13562 = CARTESIAN_POINT('',(27.8,12.9,25.5)) ;
#13563 = CARTESIAN_POINT('Origin',(27.8,25.5,25.5)) ;
#13564 = CARTESIAN_POINT('',(27.8,13.5,25.5)) ;
#13565 = CARTESIAN_POINT('Origin',(27.8,25.5,25.5)) ;
#13566 = CARTESIAN_POINT('Origin',(28.45,25.5,25.5)) ;
#13567 = CARTESIAN_POINT('',(29.1,12.9,25.5)) ;
#13568 = CARTESIAN_POINT('',(28.45,12.9,25.5)) ;
#13569 = CARTESIAN_POINT('Origin',(29.1,25.5,25.5)) ;
#13570 = CARTESIAN_POINT('Origin',(29.1,37.4,25.5)) ;
#13571 = CARTESIAN_POINT('',(29.1,13.5,25.5)) ;
#13572 = CARTESIAN_POINT('Origin',(29.1,25.5,25.5)) ;
#13573 = CARTESIAN_POINT('Origin',(29.55,25.5,25.5)) ;
#13574 = CARTESIAN_POINT('',(32.1,13.5,25.5)) ;
#13575 = CARTESIAN_POINT('Origin',(32.1,25.5,25.5)) ;
#13576 = CARTESIAN_POINT('',(29.55,13.5,25.5)) ;
#13577 = CARTESIAN_POINT('Origin',(32.1,37.5,25.5)) ;
#13578 = CARTESIAN_POINT('Origin',(29.55,25.5,25.5)) ;
#13579 = CARTESIAN_POINT('',(27.,13.5,25.5)) ;
#13580 = CARTESIAN_POINT('',(29.55,13.5,25.5)) ;
#13581 = CARTESIAN_POINT('Origin',(27.,25.5,25.5)) ;
#13582 = CARTESIAN_POINT('Origin',(27.,50.5,25.5)) ;
#13583 = CARTESIAN_POINT('',(27.,0.500000000000003,25.5)) ;
#13584 = CARTESIAN_POINT('Origin',(27.,25.5,25.5)) ;
#13585 = CARTESIAN_POINT('Origin',(27.25,25.5,25.5)) ;
#13586 = CARTESIAN_POINT('',(27.5,2.53269627492614E-15,25.5)) ;
#13587 = CARTESIAN_POINT('Origin',(27.5,25.5,25.5)) ;
#13588 = CARTESIAN_POINT('',(27.25,0.250000000000004,25.5)) ;
#13589 = CARTESIAN_POINT('Origin',(30.5,25.5,25.5)) ;
#13590 = CARTESIAN_POINT('',(33.5,0.,25.5)) ;
#13591 = CARTESIAN_POINT('Origin',(33.5,25.5,25.5)) ;
#13592 = CARTESIAN_POINT('',(30.5,0.,25.5)) ;
#13593 = CARTESIAN_POINT('Origin',(33.75,25.5,25.5)) ;
#13594 = CARTESIAN_POINT('',(33.75,0.250000000000004,25.5)) ;
#13595 = CARTESIAN_POINT('Origin',(76.75,25.5,25.5)) ;
#13596 = CARTESIAN_POINT('',(77.,10.5,25.5)) ;
#13597 = CARTESIAN_POINT('Origin',(77.,25.5,25.5)) ;
#13598 = CARTESIAN_POINT('',(76.75,10.25,25.5)) ;
#13599 = CARTESIAN_POINT('Origin',(77.,37.5,25.5)) ;
#13600 = CARTESIAN_POINT('Origin',(74.45,25.5,25.5)) ;
#13601 = CARTESIAN_POINT('',(74.45,13.5,25.5)) ;
#13602 = CARTESIAN_POINT('',(0.,0.,0.)) ;
#13603 = CARTESIAN_POINT('Origin',(33.9,20.3027651582789,17.9693127803633)) ;
#13604 = CARTESIAN_POINT('',(33.9,21.0231457651488,18.6896933872332)) ;
#13605 = CARTESIAN_POINT('',(70.1,21.0231457651488,18.6896933872332)) ;
#13606 = CARTESIAN_POINT('',(52.,21.0231457651488,18.6896933872332)) ;
#13607 = CARTESIAN_POINT('',(33.9,20.7706469832483,18.4371946053327)) ;
#13608 = CARTESIAN_POINT('',(33.9,21.29271465194,18.9592622740244)) ;
#13609 = CARTESIAN_POINT('',(70.1,20.7706469832483,18.4371946053327)) ;
#13610 = CARTESIAN_POINT('',(52.,20.7706469832483,18.4371946053327)) ;
#13611 = CARTESIAN_POINT('',(70.1,21.29271465194,18.9592622740244)) ;
#13612 = CARTESIAN_POINT('Origin',(70.1,19.6310137161517,19.6310137161517)) ;
#13613 = CARTESIAN_POINT('',(70.1,18.6896933872332,21.0231457651488)) ;
#13614 = CARTESIAN_POINT('Origin',(70.1,25.5,25.5)) ;
#13615 = CARTESIAN_POINT('',(70.1,18.4371946053327,20.7706469832483)) ;
#13616 = CARTESIAN_POINT('Origin',(70.1,25.5,25.5)) ;
#13617 = CARTESIAN_POINT('',(70.1,17.9693127803633,20.3027651582789)) ;
#13618 = CARTESIAN_POINT('Origin',(33.9,18.9592622740244,21.29271465194)) ;
#13619 = CARTESIAN_POINT('',(33.9,18.6896933872332,21.0231457651488)) ;
#13620 = CARTESIAN_POINT('',(52.,18.6896933872332,21.0231457651488)) ;
#13621 = CARTESIAN_POINT('',(33.9,18.4371946053327,20.7706469832483)) ;
#13622 = CARTESIAN_POINT('',(52.,18.4371946053327,20.7706469832483)) ;
#13623 = CARTESIAN_POINT('',(33.9,17.9693127803633,20.3027651582789)) ;
#13624 = CARTESIAN_POINT('Origin',(33.9,19.6310137161517,19.6310137161517)) ;
#13625 = CARTESIAN_POINT('Origin',(33.9,25.5,25.5)) ;
#13626 = CARTESIAN_POINT('Origin',(33.9,25.5,25.5)) ;
#13627 = CARTESIAN_POINT('Origin',(33.9,33.0306872196367,20.3027651582789)) ;
#13628 = CARTESIAN_POINT('',(33.9,32.3103066127668,21.0231457651488)) ;
#13629 = CARTESIAN_POINT('',(70.1,32.3103066127668,21.0231457651488)) ;
#13630 = CARTESIAN_POINT('',(52.,32.3103066127668,21.0231457651488)) ;
#13631 = CARTESIAN_POINT('',(33.9,32.5628053946673,20.7706469832483)) ;
#13632 = CARTESIAN_POINT('',(33.9,32.0407377259756,21.29271465194)) ;
#13633 = CARTESIAN_POINT('',(70.1,32.5628053946673,20.7706469832483)) ;
#13634 = CARTESIAN_POINT('',(52.,32.5628053946673,20.7706469832483)) ;
#13635 = CARTESIAN_POINT('',(70.1,32.0407377259756,21.29271465194)) ;
#13636 = CARTESIAN_POINT('Origin',(70.1,31.3689862838483,19.6310137161517)) ;
#13637 = CARTESIAN_POINT('',(70.1,29.9768542348512,18.6896933872332)) ;
#13638 = CARTESIAN_POINT('Origin',(70.1,25.5,25.5)) ;
#13639 = CARTESIAN_POINT('',(70.1,30.2293530167517,18.4371946053327)) ;
#13640 = CARTESIAN_POINT('Origin',(70.1,25.5,25.5)) ;
#13641 = CARTESIAN_POINT('',(70.1,30.6972348417211,17.9693127803633)) ;
#13642 = CARTESIAN_POINT('Origin',(33.9,29.70728534806,18.9592622740244)) ;
#13643 = CARTESIAN_POINT('',(33.9,29.9768542348512,18.6896933872332)) ;
#13644 = CARTESIAN_POINT('',(52.,29.9768542348512,18.6896933872332)) ;
#13645 = CARTESIAN_POINT('',(33.9,30.2293530167517,18.4371946053327)) ;
#13646 = CARTESIAN_POINT('',(52.,30.2293530167517,18.4371946053327)) ;
#13647 = CARTESIAN_POINT('',(33.9,30.6972348417211,17.9693127803633)) ;
#13648 = CARTESIAN_POINT('Origin',(33.9,31.3689862838483,19.6310137161517)) ;
#13649 = CARTESIAN_POINT('Origin',(33.9,25.5,25.5)) ;
#13650 = CARTESIAN_POINT('Origin',(33.9,25.5,25.5)) ;
#13651 = CARTESIAN_POINT('Origin',(33.9,30.6972348417211,33.0306872196367)) ;
#13652 = CARTESIAN_POINT('',(33.9,29.9768542348512,32.3103066127668)) ;
#13653 = CARTESIAN_POINT('',(70.1,29.9768542348512,32.3103066127668)) ;
#13654 = CARTESIAN_POINT('',(52.,29.9768542348512,32.3103066127668)) ;
#13655 = CARTESIAN_POINT('',(33.9,30.2293530167517,32.5628053946673)) ;
#13656 = CARTESIAN_POINT('',(33.9,29.70728534806,32.0407377259756)) ;
#13657 = CARTESIAN_POINT('',(70.1,30.2293530167517,32.5628053946673)) ;
#13658 = CARTESIAN_POINT('',(52.,30.2293530167517,32.5628053946673)) ;
#13659 = CARTESIAN_POINT('',(70.1,29.70728534806,32.0407377259756)) ;
#13660 = CARTESIAN_POINT('Origin',(70.1,31.3689862838483,31.3689862838483)) ;
#13661 = CARTESIAN_POINT('',(70.1,32.3103066127668,29.9768542348512)) ;
#13662 = CARTESIAN_POINT('Origin',(70.1,25.5,25.5)) ;
#13663 = CARTESIAN_POINT('',(70.1,32.5628053946673,30.2293530167517)) ;
#13664 = CARTESIAN_POINT('Origin',(70.1,25.5,25.5)) ;
#13665 = CARTESIAN_POINT('',(70.1,33.0306872196367,30.6972348417211)) ;
#13666 = CARTESIAN_POINT('Origin',(33.9,32.0407377259756,29.70728534806)) ;
#13667 = CARTESIAN_POINT('',(33.9,32.3103066127668,29.9768542348512)) ;
#13668 = CARTESIAN_POINT('',(52.,32.3103066127668,29.9768542348512)) ;
#13669 = CARTESIAN_POINT('',(33.9,32.5628053946673,30.2293530167517)) ;
#13670 = CARTESIAN_POINT('',(52.,32.5628053946673,30.2293530167517)) ;
#13671 = CARTESIAN_POINT('',(33.9,33.0306872196367,30.6972348417211)) ;
#13672 = CARTESIAN_POINT('Origin',(33.9,31.3689862838483,31.3689862838483)) ;
#13673 = CARTESIAN_POINT('Origin',(33.9,25.5,25.5)) ;
#13674 = CARTESIAN_POINT('Origin',(33.9,25.5,25.5)) ;
#13675 = CARTESIAN_POINT('Origin',(33.9,17.9693127803633,30.6972348417211)) ;
#13676 = CARTESIAN_POINT('',(33.9,18.6896933872332,29.9768542348512)) ;
#13677 = CARTESIAN_POINT('',(70.1,18.6896933872332,29.9768542348512)) ;
#13678 = CARTESIAN_POINT('',(52.,18.6896933872332,29.9768542348512)) ;
#13679 = CARTESIAN_POINT('',(33.9,18.4371946053327,30.2293530167517)) ;
#13680 = CARTESIAN_POINT('',(33.9,18.9592622740244,29.70728534806)) ;
#13681 = CARTESIAN_POINT('',(70.1,18.4371946053327,30.2293530167517)) ;
#13682 = CARTESIAN_POINT('',(52.,18.4371946053327,30.2293530167517)) ;
#13683 = CARTESIAN_POINT('',(70.1,18.9592622740244,29.70728534806)) ;
#13684 = CARTESIAN_POINT('Origin',(70.1,19.6310137161517,31.3689862838483)) ;
#13685 = CARTESIAN_POINT('',(70.1,21.0231457651488,32.3103066127668)) ;
#13686 = CARTESIAN_POINT('Origin',(70.1,25.5,25.5)) ;
#13687 = CARTESIAN_POINT('',(70.1,20.7706469832483,32.5628053946673)) ;
#13688 = CARTESIAN_POINT('Origin',(70.1,25.5,25.5)) ;
#13689 = CARTESIAN_POINT('',(70.1,20.3027651582789,33.0306872196367)) ;
#13690 = CARTESIAN_POINT('Origin',(33.9,21.29271465194,32.0407377259756)) ;
#13691 = CARTESIAN_POINT('',(33.9,21.0231457651488,32.3103066127668)) ;
#13692 = CARTESIAN_POINT('',(52.,21.0231457651488,32.3103066127668)) ;
#13693 = CARTESIAN_POINT('',(33.9,20.7706469832483,32.5628053946673)) ;
#13694 = CARTESIAN_POINT('',(52.,20.7706469832483,32.5628053946673)) ;
#13695 = CARTESIAN_POINT('',(33.9,20.3027651582789,33.0306872196367)) ;
#13696 = CARTESIAN_POINT('Origin',(33.9,19.6310137161517,31.3689862838483)) ;
#13697 = CARTESIAN_POINT('Origin',(33.9,25.5,25.5)) ;
#13698 = CARTESIAN_POINT('Origin',(33.9,25.5,25.5)) ;
#13699 = CARTESIAN_POINT('Origin',(52.,25.5,25.5)) ;
#13700 = CARTESIAN_POINT('',(71.,17.35,25.5)) ;
#13701 = CARTESIAN_POINT('Origin',(71.,25.5,25.5)) ;
#13702 = CARTESIAN_POINT('',(33.,17.35,25.5)) ;
#13703 = CARTESIAN_POINT('',(52.,17.35,25.5)) ;
#13704 = CARTESIAN_POINT('Origin',(33.,25.5,25.5)) ;
#13705 = CARTESIAN_POINT('Origin',(33.,34.,25.5)) ;
#13706 = CARTESIAN_POINT('',(33.,17.,25.5)) ;
#13707 = CARTESIAN_POINT('Origin',(33.,25.5,25.5)) ;
#13708 = CARTESIAN_POINT('Origin',(52.,25.5,25.5)) ;
#13709 = CARTESIAN_POINT('',(71.,17.,25.5)) ;
#13710 = CARTESIAN_POINT('Origin',(71.,25.5,25.5)) ;
#13711 = CARTESIAN_POINT('',(52.,17.,25.5)) ;
#13712 = CARTESIAN_POINT('Origin',(71.,33.65,25.5)) ;
#13713 = CARTESIAN_POINT('',(0.,0.,0.)) ;
#13714 = CARTESIAN_POINT('Origin',(35.75,31.1568542494924,31.1568542)) ;
#13715 = CARTESIAN_POINT('',(35.75,31.1568542494924,32.7443542)) ;
#13716 = CARTESIAN_POINT('',(35.75,31.1568542494924,29.5693542)) ;
#13717 = CARTESIAN_POINT('Origin',(35.75,31.1568542494924,31.1568542)) ;
#13718 = CARTESIAN_POINT('',(0.,0.,0.)) ;
#13719 = CARTESIAN_POINT('Origin',(29.6,39.642135623731,39.642135623731)) ;
#13720 = CARTESIAN_POINT('',(29.1741303078758,39.6408187757763,41.5983047332171)) ;
#13721 = CARTESIAN_POINT('',(29.2758696921242,39.6403302138731,41.5978361791329)) ;
#13722 = CARTESIAN_POINT('',(29.6,39.642135623731,41.596135623731)) ;
#13723 = CARTESIAN_POINT('',(29.4,37.887097212946,38.7795589530206)) ;
#13724 = CARTESIAN_POINT('Ctrl Pts',(29.1741303078758,39.6408187757763,41.5983047332171)) ;
#13725 = CARTESIAN_POINT('Ctrl Pts',(29.178358479461,39.5668972107545,41.5988463683251)) ;
#13726 = CARTESIAN_POINT('Ctrl Pts',(29.1825866510463,39.4930348242883,41.5950187173956)) ;
#13727 = CARTESIAN_POINT('Ctrl Pts',(29.1868148226315,39.4196968033455,41.5866345034286)) ;
#13728 = CARTESIAN_POINT('Ctrl Pts',(29.2237530942682,38.7789991201355,41.5133880973328)) ;
#13729 = CARTESIAN_POINT('Ctrl Pts',(29.260691365905,38.1783218958328,41.0923771345517)) ;
#13730 = CARTESIAN_POINT('Ctrl Pts',(29.2976296375417,37.8905206264674,40.5150612002977)) ;
#13731 = CARTESIAN_POINT('Ctrl Pts',(29.3317530916944,37.6246507580315,39.9817386342627)) ;
#13732 = CARTESIAN_POINT('Ctrl Pts',(29.3658765458472,37.6257893479619,39.3150253464114)) ;
#13733 = CARTESIAN_POINT('Ctrl Pts',(29.4,37.8858801137886,38.7785081419809)) ;
#13734 = CARTESIAN_POINT('',(29.4,37.8883143121033,40.5036614834013)) ;
#13735 = CARTESIAN_POINT('Origin',(29.4,39.642135623731,39.642135623731)) ;
#13736 = CARTESIAN_POINT('Ctrl Pts',(29.4,37.8883143121033,40.5036614834013)) ;
#13737 = CARTESIAN_POINT('Ctrl Pts',(29.3630617283633,38.1739593715505,41.0851534806482)) ;
#13738 = CARTESIAN_POINT('Ctrl Pts',(29.3261234567266,38.7692045105899,41.5084274781235)) ;
#13739 = CARTESIAN_POINT('Ctrl Pts',(29.2891851850899,39.4085096414219,41.5850281011346)) ;
#13740 = CARTESIAN_POINT('Ctrl Pts',(29.2847466874347,39.4853284582867,41.5942324214928)) ;
#13741 = CARTESIAN_POINT('Ctrl Pts',(29.2803081897794,39.5627834306131,41.5984313355494)) ;
#13742 = CARTESIAN_POINT('Ctrl Pts',(29.2758696921242,39.6403302138731,41.5978361791329)) ;
#13743 = CARTESIAN_POINT('Origin',(29.6,39.642135623731,39.642135623731)) ;
#13744 = CARTESIAN_POINT('',(28.4741303078758,39.6414297915345,41.5932509341168)) ;
#13745 = CARTESIAN_POINT('',(28.5758696921242,39.6414773978913,41.5932079635623)) ;
#13746 = CARTESIAN_POINT('',(29.6,39.642135623731,41.596135623731)) ;
#13747 = CARTESIAN_POINT('Ctrl Pts',(28.4741303078758,39.6414297915345,41.5932509341168)) ;
#13748 = CARTESIAN_POINT('Ctrl Pts',(28.4900621829741,39.3610188002016,41.5941645620992)) ;
#13749 = CARTESIAN_POINT('Ctrl Pts',(28.5059940580724,39.0809590371883,41.5376795052535)) ;
#13750 = CARTESIAN_POINT('Ctrl Pts',(28.5219259331707,38.8279927600939,41.4219659840985)) ;
#13751 = CARTESIAN_POINT('Ctrl Pts',(28.5588642048074,38.241486965855,41.1536825930919)) ;
#13752 = CARTESIAN_POINT('Ctrl Pts',(28.5958024764441,37.8006223692225,40.5670162335662)) ;
#13753 = CARTESIAN_POINT('Ctrl Pts',(28.6327407480808,37.7060808628922,39.9290270322568)) ;
#13754 = CARTESIAN_POINT('Ctrl Pts',(28.6696790197175,37.611539356562,39.2910378309475)) ;
#13755 = CARTESIAN_POINT('Ctrl Pts',(28.7066172913542,37.8633209405341,38.6017257878545)) ;
#13756 = CARTESIAN_POINT('Ctrl Pts',(28.7435555629909,38.3468275454814,38.1748867110876)) ;
#13757 = CARTESIAN_POINT('Ctrl Pts',(28.7804938346277,38.8303341504287,37.7480476343208)) ;
#13758 = CARTESIAN_POINT('Ctrl Pts',(28.8174321062644,39.5455657763513,37.58368152388)) ;
#13759 = CARTESIAN_POINT('Ctrl Pts',(28.8543703779011,40.16689692944,37.7565991948941)) ;
#13760 = CARTESIAN_POINT('Ctrl Pts',(28.8913086495378,40.7882280825286,37.9295168659081)) ;
#13761 = CARTESIAN_POINT('Ctrl Pts',(28.9282469211745,41.3156587627833,38.4397183183768)) ;
#13762 = CARTESIAN_POINT('Ctrl Pts',(28.9651851928112,41.5091643242028,39.0549731841945)) ;
#13763 = CARTESIAN_POINT('Ctrl Pts',(29.002123464448,41.7026698856222,39.6702280500122)) ;
#13764 = CARTESIAN_POINT('Ctrl Pts',(29.0390617360846,41.5622503282064,40.3905363291788)) ;
#13765 = CARTESIAN_POINT('Ctrl Pts',(29.0760000077214,41.1516814784397,40.8879495440568)) ;
#13766 = CARTESIAN_POINT('Ctrl Pts',(29.1087101077728,40.7881087513245,41.3284259200389)) ;
#13767 = CARTESIAN_POINT('Ctrl Pts',(29.1414202078243,40.212692868176,41.5941145204462)) ;
#13768 = CARTESIAN_POINT('Ctrl Pts',(29.1741303078758,39.6408187757763,41.5983047332171)) ;
#13769 = CARTESIAN_POINT('Ctrl Pts',(29.2758696921242,39.6403302138731,41.5978361791329)) ;
#13770 = CARTESIAN_POINT('Ctrl Pts',(29.2433699181427,40.2081468772396,41.5934782971368)) ;
#13771 = CARTESIAN_POINT('Ctrl Pts',(29.2108701441612,40.7808860108025,41.3320849172391)) ;
#13772 = CARTESIAN_POINT('Ctrl Pts',(29.1783703701797,41.1448464448315,40.8966231887847)) ;
#13773 = CARTESIAN_POINT('Ctrl Pts',(29.141432098543,41.5585129947845,40.4016904048769)) ;
#13774 = CARTESIAN_POINT('Ctrl Pts',(29.1044938269063,41.7024809720658,39.6818975885143)) ;
#13775 = CARTESIAN_POINT('Ctrl Pts',(29.0675555552696,41.512330041934,39.0654838455824)) ;
#13776 = CARTESIAN_POINT('Ctrl Pts',(29.0306172836329,41.3221791118021,38.4490701026506)) ;
#13777 = CARTESIAN_POINT('Ctrl Pts',(28.9936790119962,40.7979092742571,37.9360354331494)) ;
#13778 = CARTESIAN_POINT('Ctrl Pts',(28.9567407403594,40.1776331119795,37.7596379549628)) ;
#13779 = CARTESIAN_POINT('Ctrl Pts',(28.9198024687227,39.5573569497018,37.5832404767762)) ;
#13780 = CARTESIAN_POINT('Ctrl Pts',(28.882864197086,38.8410744626915,37.7434801899042)) ;
#13781 = CARTESIAN_POINT('Ctrl Pts',(28.8459259254493,38.3551253306134,38.1675558119185)) ;
#13782 = CARTESIAN_POINT('Ctrl Pts',(28.8089876538126,37.8691761985354,38.5916314339327)) ;
#13783 = CARTESIAN_POINT('Ctrl Pts',(28.7720493821759,37.6135604213898,39.2795429648331)) ;
#13784 = CARTESIAN_POINT('Ctrl Pts',(28.7351111105392,37.7045035108508,39.9180665126644)) ;
#13785 = CARTESIAN_POINT('Ctrl Pts',(28.6981728389025,37.7954466003119,40.5565900604957)) ;
#13786 = CARTESIAN_POINT('Ctrl Pts',(28.6612345672657,38.2329485563797,41.1457256252577)) ;
#13787 = CARTESIAN_POINT('Ctrl Pts',(28.624296295629,38.817917278673,41.4173218967017)) ;
#13788 = CARTESIAN_POINT('Ctrl Pts',(28.6081540944608,39.0735514048515,41.5360107648035)) ;
#13789 = CARTESIAN_POINT('Ctrl Pts',(28.5920118932925,39.357347727632,41.5940581457679)) ;
#13790 = CARTESIAN_POINT('Ctrl Pts',(28.5758696921242,39.6414773978913,41.5932079635623)) ;
#13791 = CARTESIAN_POINT('Origin',(29.6,39.642135623731,39.642135623731)) ;
#13792 = CARTESIAN_POINT('',(27.7741303078758,39.6438916302392,41.5958037900958)) ;
#13793 = CARTESIAN_POINT('',(27.8758696921242,39.6438946340221,41.5959129847908)) ;
#13794 = CARTESIAN_POINT('',(29.6,39.642135623731,41.596135623731)) ;
#13795 = CARTESIAN_POINT('Ctrl Pts',(27.7741303078758,39.6438916302392,41.5958037900958)) ;
#13796 = CARTESIAN_POINT('Ctrl Pts',(27.8017658864871,39.1590917620955,41.5914733218518)) ;
#13797 = CARTESIAN_POINT('Ctrl Pts',(27.8294014650985,38.6713775391436,41.4087948654502)) ;
#13798 = CARTESIAN_POINT('Ctrl Pts',(27.8570370437098,38.3164063634699,41.0819502323136)) ;
#13799 = CARTESIAN_POINT('Ctrl Pts',(27.8939753153465,37.8419447321562,40.6450831049201)) ;
#13800 = CARTESIAN_POINT('Ctrl Pts',(27.9309135869832,37.6046356518907,39.9506553949681)) ;
#13801 = CARTESIAN_POINT('Ctrl Pts',(27.96785185862,37.7125071897698,39.3147855252961)) ;
#13802 = CARTESIAN_POINT('Ctrl Pts',(28.0047901302567,37.820378727649,38.6789156556241)) ;
#13803 = CARTESIAN_POINT('Ctrl Pts',(28.0417284018934,38.2734308836729,38.1016036262322)) ;
#13804 = CARTESIAN_POINT('Ctrl Pts',(28.0786666735301,38.8654248336815,37.8456544202854)) ;
#13805 = CARTESIAN_POINT('Ctrl Pts',(28.1156049451668,39.4574187836902,37.5897052143387)) ;
#13806 = CARTESIAN_POINT('Ctrl Pts',(28.1525432168035,40.1883545276836,37.655118831837)) ;
#13807 = CARTESIAN_POINT('Ctrl Pts',(28.1894814884402,40.72549377371,38.0121173915036)) ;
#13808 = CARTESIAN_POINT('Ctrl Pts',(28.226419760077,41.2626330197364,38.3691159511701)) ;
#13809 = CARTESIAN_POINT('Ctrl Pts',(28.2633580317137,41.6059757677957,39.0176994530047)) ;
#13810 = CARTESIAN_POINT('Ctrl Pts',(28.3002963033504,41.5992261455199,39.6626190814621)) ;
#13811 = CARTESIAN_POINT('Ctrl Pts',(28.3372345749871,41.5924765232442,40.3075387099194)) ;
#13812 = CARTESIAN_POINT('Ctrl Pts',(28.3741728466238,41.2356345306335,40.9487944649996)) ;
#13813 = CARTESIAN_POINT('Ctrl Pts',(28.4111111182605,40.6911400384056,41.294472131296)) ;
#13814 = CARTESIAN_POINT('Ctrl Pts',(28.4321175147989,40.3814918954385,41.4910552904679)) ;
#13815 = CARTESIAN_POINT('Ctrl Pts',(28.4531239113374,40.0111555420393,41.5920463030505)) ;
#13816 = CARTESIAN_POINT('Ctrl Pts',(28.4741303078758,39.6414297915345,41.5932509341168)) ;
#13817 = CARTESIAN_POINT('Ctrl Pts',(28.5758696921242,39.6414773978913,41.5932079635623)) ;
#13818 = CARTESIAN_POINT('Ctrl Pts',(28.5550736216558,40.007522931787,41.5921126699976)) ;
#13819 = CARTESIAN_POINT('Ctrl Pts',(28.5342775511873,40.3741217319919,41.4932634125623)) ;
#13820 = CARTESIAN_POINT('Ctrl Pts',(28.5134814807189,40.6817691599538,41.3003891117333)) ;
#13821 = CARTESIAN_POINT('Ctrl Pts',(28.4765432090822,41.2282168304228,40.9578030771951)) ;
#13822 = CARTESIAN_POINT('Ctrl Pts',(28.4396049374455,41.5886766828423,40.3185740299928)) ;
#13823 = CARTESIAN_POINT('Ctrl Pts',(28.4026666658088,41.5990767145884,39.6737018167311)) ;
#13824 = CARTESIAN_POINT('Ctrl Pts',(28.365728394172,41.6094767463344,39.0288296034693)) ;
#13825 = CARTESIAN_POINT('Ctrl Pts',(28.3287901225353,41.2698169574072,38.3783142241481)) ;
#13826 = CARTESIAN_POINT('Ctrl Pts',(28.2918518508986,40.7347092510962,38.0182798055956)) ;
#13827 = CARTESIAN_POINT('Ctrl Pts',(28.2549135792619,40.1996015447852,37.658245387043)) ;
#13828 = CARTESIAN_POINT('Ctrl Pts',(28.2179753076252,39.4690459210904,37.5886919292591)) ;
#13829 = CARTESIAN_POINT('Ctrl Pts',(28.1810370359885,38.8756113406825,37.841283921041)) ;
#13830 = CARTESIAN_POINT('Ctrl Pts',(28.1440987643517,38.2821767602745,38.0938759128229)) ;
#13831 = CARTESIAN_POINT('Ctrl Pts',(28.107160492715,37.8258632231532,38.6686133541705)) ;
#13832 = CARTESIAN_POINT('Ctrl Pts',(28.0702222210783,37.7143923484776,39.3038622372428)) ;
#13833 = CARTESIAN_POINT('Ctrl Pts',(28.0332839494416,37.6029214738019,39.939111120315)) ;
#13834 = CARTESIAN_POINT('Ctrl Pts',(27.9963456778049,37.8362932615717,40.634871445112)) ;
#13835 = CARTESIAN_POINT('Ctrl Pts',(27.9594074061682,38.3082729142534,41.0744186707252)) ;
#13836 = CARTESIAN_POINT('Ctrl Pts',(27.9315615014869,38.6640746298656,41.4057712111943)) ;
#13837 = CARTESIAN_POINT('Ctrl Pts',(27.9037155968056,39.1554746557266,41.5915205741414)) ;
#13838 = CARTESIAN_POINT('Ctrl Pts',(27.8758696921242,39.6438946340221,41.5959129847908)) ;
#13839 = CARTESIAN_POINT('Origin',(29.6,39.642135623731,39.642135623731)) ;
#13840 = CARTESIAN_POINT('',(27.0741303078758,39.6413906238265,41.5989800840457)) ;
#13841 = CARTESIAN_POINT('',(27.1758696921242,39.6413307831041,41.5989199275014)) ;
#13842 = CARTESIAN_POINT('',(29.6,39.642135623731,41.596135623731)) ;
#13843 = CARTESIAN_POINT('Ctrl Pts',(27.0741303078758,39.6413906238265,41.5989800840457)) ;
#13844 = CARTESIAN_POINT('Ctrl Pts',(27.0765313183635,39.5994478954968,41.5991853621116)) ;
#13845 = CARTESIAN_POINT('Ctrl Pts',(27.0789323288512,39.5575174495919,41.597952947044)) ;
#13846 = CARTESIAN_POINT('Ctrl Pts',(27.0813333393388,39.5156825771046,41.5952443691905)) ;
#13847 = CARTESIAN_POINT('Ctrl Pts',(27.1182716109756,38.872075274369,41.5535743369209)) ;
#13848 = CARTESIAN_POINT('Ctrl Pts',(27.1552098826123,38.2510884686797,41.1625233076746)) ;
#13849 = CARTESIAN_POINT('Ctrl Pts',(27.192148154249,37.9354087484862,40.60010614448)) ;
#13850 = CARTESIAN_POINT('Ctrl Pts',(27.2290864258857,37.6197290282927,40.0376889812855)) ;
#13851 = CARTESIAN_POINT('Ctrl Pts',(27.2660246975224,37.6093563935951,39.3039056841426)) ;
#13852 = CARTESIAN_POINT('Ctrl Pts',(27.3029629691591,37.909012689149,38.7327902352957)) ;
#13853 = CARTESIAN_POINT('Ctrl Pts',(27.3399012407958,38.2086689847029,38.1616747864487)) ;
#13854 = CARTESIAN_POINT('Ctrl Pts',(27.3768395124325,38.8183542105085,37.7532271858975)) ;
#13855 = CARTESIAN_POINT('Ctrl Pts',(27.4137777840693,39.4605265067115,37.6933815922678)) ;
#13856 = CARTESIAN_POINT('Ctrl Pts',(27.450716055706,40.1026988029146,37.6335359986382)) ;
#13857 = CARTESIAN_POINT('Ctrl Pts',(27.4876543273427,40.7773581695152,37.92229241193)) ;
#13858 = CARTESIAN_POINT('Ctrl Pts',(27.5245925989794,41.1773851027979,38.4282026819346)) ;
#13859 = CARTESIAN_POINT('Ctrl Pts',(27.5615308706161,41.5774120360807,38.9341129519391)) ;
#13860 = CARTESIAN_POINT('Ctrl Pts',(27.5984691422528,41.7028065360457,39.6571770786564)) ;
#13861 = CARTESIAN_POINT('Ctrl Pts',(27.6354074138895,41.4964863399443,40.2682406826823)) ;
#13862 = CARTESIAN_POINT('Ctrl Pts',(27.6723456855263,41.2901661438429,40.8793042867082)) ;
#13863 = CARTESIAN_POINT('Ctrl Pts',(27.709283957163,40.7521312516751,41.3783673680427)) ;
#13864 = CARTESIAN_POINT('Ctrl Pts',(27.7462222287997,40.1273067144102,41.5382456362924)) ;
#13865 = CARTESIAN_POINT('Ctrl Pts',(27.7555249218251,39.9699482185376,41.5785100662469)) ;
#13866 = CARTESIAN_POINT('Ctrl Pts',(27.7648276148504,39.8070850417288,41.5972615130296)) ;
#13867 = CARTESIAN_POINT('Ctrl Pts',(27.7741303078758,39.6438916302392,41.5958037900958)) ;
#13868 = CARTESIAN_POINT('Ctrl Pts',(27.8758696921242,39.6438946340221,41.5959129847908)) ;
#13869 = CARTESIAN_POINT('Ctrl Pts',(27.8667773251688,39.8033756680138,41.5973472139854)) ;
#13870 = CARTESIAN_POINT('Ctrl Pts',(27.8576849582135,39.9625389747718,41.5794454958518)) ;
#13871 = CARTESIAN_POINT('Ctrl Pts',(27.8485925912581,40.1165601657379,41.5409631187002)) ;
#13872 = CARTESIAN_POINT('Ctrl Pts',(27.8116543196213,40.7422802469475,41.3846262146325)) ;
#13873 = CARTESIAN_POINT('Ctrl Pts',(27.7747160479846,41.2831328917734,40.8886182800675)) ;
#13874 = CARTESIAN_POINT('Ctrl Pts',(27.7377777763479,41.4929105802845,40.2787329662382)) ;
#13875 = CARTESIAN_POINT('Ctrl Pts',(27.7008395047112,41.7026882687956,39.6688476524089)) ;
#13876 = CARTESIAN_POINT('Ctrl Pts',(27.6639012330745,41.5813910009921,38.9450849593151)) ;
#13877 = CARTESIAN_POINT('Ctrl Pts',(27.6269629614378,41.1842357746265,38.436917203995)) ;
#13878 = CARTESIAN_POINT('Ctrl Pts',(27.5900246898011,40.7870805482609,37.9287494486749)) ;
#13879 = CARTESIAN_POINT('Ctrl Pts',(27.5530864181643,40.1140673633333,37.6361766311283)) ;
#13880 = CARTESIAN_POINT('Ctrl Pts',(27.5161481465276,39.4715664044991,37.6923842435544)) ;
#13881 = CARTESIAN_POINT('Ctrl Pts',(27.4792098748909,38.8290654456649,37.7485918559805)) ;
#13882 = CARTESIAN_POINT('Ctrl Pts',(27.4422716032542,38.2170767129241,38.1535798983792)) ;
#13883 = CARTESIAN_POINT('Ctrl Pts',(27.4053333316175,37.914190642964,38.7229890613612)) ;
#13884 = CARTESIAN_POINT('Ctrl Pts',(27.3683950599808,37.6113045730038,39.2923982243431)) ;
#13885 = CARTESIAN_POINT('Ctrl Pts',(27.331456788344,37.6175211658244,40.0262285079083)) ;
#13886 = CARTESIAN_POINT('Ctrl Pts',(27.2945185167073,37.9300105111892,40.5904245487143)) ;
#13887 = CARTESIAN_POINT('Ctrl Pts',(27.2575802450706,38.2424998565541,41.1546205895204)) ;
#13888 = CARTESIAN_POINT('Ctrl Pts',(27.2206419734339,38.8612619544631,41.5491823875673)) ;
#13889 = CARTESIAN_POINT('Ctrl Pts',(27.1837037017972,39.5046229441121,41.5944968980767)) ;
#13890 = CARTESIAN_POINT('Ctrl Pts',(27.1810923652396,39.5501050957558,41.5977003895408)) ;
#13891 = CARTESIAN_POINT('Ctrl Pts',(27.1784810286819,39.5957101859526,41.599158438298)) ;
#13892 = CARTESIAN_POINT('Ctrl Pts',(27.1758696921242,39.6413307831041,41.5989199275014)) ;
#13893 = CARTESIAN_POINT('Origin',(29.6,39.642135623731,39.642135623731)) ;
#13894 = CARTESIAN_POINT('',(26.3741303078758,39.6409887519309,41.5937162339903)) ;
#13895 = CARTESIAN_POINT('',(26.4758696921242,39.6410353087582,41.5936514180137)) ;
#13896 = CARTESIAN_POINT('',(29.6,39.642135623731,41.596135623731)) ;
#13897 = CARTESIAN_POINT('Ctrl Pts',(26.3741303078758,39.6409887519309,41.5937162339903)) ;
#13898 = CARTESIAN_POINT('Ctrl Pts',(26.3882350218765,39.3928854212053,41.5950519462106)) ;
#13899 = CARTESIAN_POINT('Ctrl Pts',(26.4023397358772,39.1452370348786,41.5511579885616)) ;
#13900 = CARTESIAN_POINT('Ctrl Pts',(26.416444449878,38.9165146177542,41.4598535061621)) ;
#13901 = CARTESIAN_POINT('Ctrl Pts',(26.4533827215147,38.3175226231131,41.2207398472572)) ;
#13902 = CARTESIAN_POINT('Ctrl Pts',(26.4903209931514,37.848333022201,40.6564645263628)) ;
#13903 = CARTESIAN_POINT('Ctrl Pts',(26.5272592647882,37.7225310407902,40.0238978397713)) ;
#13904 = CARTESIAN_POINT('Ctrl Pts',(26.5641975364249,37.5967290593794,39.3913311531798)) ;
#13905 = CARTESIAN_POINT('Ctrl Pts',(26.6011358080616,37.8143146974699,38.6904731008914)) ;
#13906 = CARTESIAN_POINT('Ctrl Pts',(26.6380740796983,38.2762382797088,38.2403693843094)) ;
#13907 = CARTESIAN_POINT('Ctrl Pts',(26.675012351335,38.7381618619478,37.7902656677275)) ;
#13908 = CARTESIAN_POINT('Ctrl Pts',(26.7119506229717,39.4444233883352,37.5909162868521)) ;
#13909 = CARTESIAN_POINT('Ctrl Pts',(26.7488888946084,40.0735173795759,37.7330693794226)) ;
#13910 = CARTESIAN_POINT('Ctrl Pts',(26.7858271662451,40.7026113708165,37.8752224719931)) ;
#13911 = CARTESIAN_POINT('Ctrl Pts',(26.8227654378819,41.2545378269104,38.3588780380096)) ;
#13912 = CARTESIAN_POINT('Ctrl Pts',(26.8597037095186,41.4780479210239,38.9638656323544)) ;
#13913 = CARTESIAN_POINT('Ctrl Pts',(26.8966419811553,41.7015580151375,39.5688532266993)) ;
#13914 = CARTESIAN_POINT('Ctrl Pts',(26.933580252792,41.5966517472707,40.2951728493725)) ;
#13915 = CARTESIAN_POINT('Ctrl Pts',(26.9705185244287,41.2110847134464,40.8121881430627)) ;
#13916 = CARTESIAN_POINT('Ctrl Pts',(27.0050557855777,40.8505797751371,41.2955971230993)) ;
#13917 = CARTESIAN_POINT('Ctrl Pts',(27.0395930467267,40.244714503106,41.5960272680518)) ;
#13918 = CARTESIAN_POINT('Ctrl Pts',(27.0741303078758,39.6413906238265,41.5989800840457)) ;
#13919 = CARTESIAN_POINT('Ctrl Pts',(27.1758696921242,39.6413307831041,41.5989199275014)) ;
#13920 = CARTESIAN_POINT('Ctrl Pts',(27.1415427570452,40.2410295358732,41.5957846194131)) ;
#13921 = CARTESIAN_POINT('Ctrl Pts',(27.1072158219661,40.8434078942437,41.2994834007345)) ;
#13922 = CARTESIAN_POINT('Ctrl Pts',(27.0728888868871,41.2044328480336,40.8210553245055)) ;
#13923 = CARTESIAN_POINT('Ctrl Pts',(27.0359506152503,41.5929218809174,40.306232017453)) ;
#13924 = CARTESIAN_POINT('Ctrl Pts',(26.9990123436136,41.701940065296,39.5805181803762)) ;
#13925 = CARTESIAN_POINT('Ctrl Pts',(26.9620740719769,41.4818599702313,38.9742744028971)) ;
#13926 = CARTESIAN_POINT('Ctrl Pts',(26.9251358003402,41.2617798751665,38.3680306254179)) ;
#13927 = CARTESIAN_POINT('Ctrl Pts',(26.8881975287035,40.7126015006585,37.8812569075366)) ;
#13928 = CARTESIAN_POINT('Ctrl Pts',(26.8512592570668,40.0843226884506,37.735543144862)) ;
#13929 = CARTESIAN_POINT('Ctrl Pts',(26.8143209854301,39.4560438762427,37.5898293821874)) ;
#13930 = CARTESIAN_POINT('Ctrl Pts',(26.7773827137934,38.748664626335,37.7851755747196)) ;
#13931 = CARTESIAN_POINT('Ctrl Pts',(26.7404444421566,38.2841992294164,38.2326559221377)) ;
#13932 = CARTESIAN_POINT('Ctrl Pts',(26.7035061705199,37.8197338324979,38.6801362695557)) ;
#13933 = CARTESIAN_POINT('Ctrl Pts',(26.6665678988832,37.5981822885685,39.3797507718596)) ;
#13934 = CARTESIAN_POINT('Ctrl Pts',(26.6296296272465,37.7203996390852,40.0130198185474)) ;
#13935 = CARTESIAN_POINT('Ctrl Pts',(26.5926913556098,37.8426169896019,40.6462888652352)) ;
#13936 = CARTESIAN_POINT('Ctrl Pts',(26.5557530839731,38.3086032345646,41.213212456307)) ;
#13937 = CARTESIAN_POINT('Ctrl Pts',(26.5188148123364,38.9062313848036,41.4557147457038)) ;
#13938 = CARTESIAN_POINT('Ctrl Pts',(26.5044997722657,39.1378359114635,41.5496939666077)) ;
#13939 = CARTESIAN_POINT('Ctrl Pts',(26.490184732195,39.3892113251267,41.5949493644748)) ;
#13940 = CARTESIAN_POINT('Ctrl Pts',(26.4758696921242,39.6410353087582,41.5936514180137)) ;
#13941 = CARTESIAN_POINT('Origin',(29.6,39.642135623731,39.642135623731)) ;
#13942 = CARTESIAN_POINT('',(25.6741303078758,39.6437755905604,41.5948983538003)) ;
#13943 = CARTESIAN_POINT('',(25.7758696921242,39.6437968858784,41.5949974857067)) ;
#13944 = CARTESIAN_POINT('',(29.6,39.642135623731,41.596135623731)) ;
#13945 = CARTESIAN_POINT('Ctrl Pts',(25.6741303078758,39.6437755905604,41.5948983538003)) ;
#13946 = CARTESIAN_POINT('Ctrl Pts',(25.6999387253896,39.1904952337914,41.5912583415157)) ;
#13947 = CARTESIAN_POINT('Ctrl Pts',(25.7257471429034,38.734936108021,41.4339712696229)) ;
#13948 = CARTESIAN_POINT('Ctrl Pts',(25.7515555604172,38.3888234438755,41.1454096254523)) ;
#13949 = CARTESIAN_POINT('Ctrl Pts',(25.7884938320539,37.8934500410593,40.732406062153)) ;
#13950 = CARTESIAN_POINT('Ctrl Pts',(25.8254321036906,37.6222748349651,40.0504899918325)) ;
#13951 = CARTESIAN_POINT('Ctrl Pts',(25.8623703753273,37.6987426280783,39.4100843171763)) ;
#13952 = CARTESIAN_POINT('Ctrl Pts',(25.899308646964,37.7752104211915,38.76967864252)) ;
#13953 = CARTESIAN_POINT('Ctrl Pts',(25.9362469186007,38.199321213512,38.170783363528)) ;
#13954 = CARTESIAN_POINT('Ctrl Pts',(25.9731851902374,38.7780106252096,37.8860285280915)) ;
#13955 = CARTESIAN_POINT('Ctrl Pts',(26.0101234618742,39.3567000369072,37.6012736926549)) ;
#13956 = CARTESIAN_POINT('Ctrl Pts',(26.0470617335109,40.0899680679818,37.6306593007738)) ;
#13957 = CARTESIAN_POINT('Ctrl Pts',(26.0840000051476,40.6440152956615,37.9608083898478)) ;
#13958 = CARTESIAN_POINT('Ctrl Pts',(26.1209382767843,41.1980625233412,38.2909574789218)) ;
#13959 = CARTESIAN_POINT('Ctrl Pts',(26.157876548421,41.572888947626,38.9218700489509)) ;
#13960 = CARTESIAN_POINT('Ctrl Pts',(26.1948148200577,41.5978654959725,39.5663410906184)) ;
#13961 = CARTESIAN_POINT('Ctrl Pts',(26.2317530916944,41.622842044319,40.2108121322859)) ;
#13962 = CARTESIAN_POINT('Ctrl Pts',(26.2686913633312,41.2979687167271,40.8688416455917)) ;
#13963 = CARTESIAN_POINT('Ctrl Pts',(26.3056296349679,40.7711348587462,41.2408804037869)) ;
#13964 = CARTESIAN_POINT('Ctrl Pts',(26.3284631926038,40.4454701557764,41.4708578242687)) ;
#13965 = CARTESIAN_POINT('Ctrl Pts',(26.3512967502398,40.0426333156918,41.5915539028743)) ;
#13966 = CARTESIAN_POINT('Ctrl Pts',(26.3741303078758,39.6409887519309,41.5937162339903)) ;
#13967 = CARTESIAN_POINT('Ctrl Pts',(26.4758696921242,39.6410353087582,41.5936514180137)) ;
#13968 = CARTESIAN_POINT('Ctrl Pts',(26.4532464605582,40.0390133980566,41.5916001667979)) ;
#13969 = CARTESIAN_POINT('Ctrl Pts',(26.4306232289922,40.4381118389579,41.4732769454704)) ;
#13970 = CARTESIAN_POINT('Ctrl Pts',(26.4079999974262,40.7620620933454,41.2472490101119)) ;
#13971 = CARTESIAN_POINT('Ctrl Pts',(26.3710617257895,41.2909945961329,40.8781999974013)) ;
#13972 = CARTESIAN_POINT('Ctrl Pts',(26.3341234541528,41.6195895461926,40.2220209842581)) ;
#13973 = CARTESIAN_POINT('Ctrl Pts',(26.2971851825161,41.5982634351316,39.5774188098299)) ;
#13974 = CARTESIAN_POINT('Ctrl Pts',(26.2602469108794,41.5769373240706,38.9328166354017)) ;
#13975 = CARTESIAN_POINT('Ctrl Pts',(26.2233086392427,41.2056901518889,38.2997912996883)) ;
#13976 = CARTESIAN_POINT('Ctrl Pts',(26.1863703676059,40.6535216383902,37.966509588522)) ;
#13977 = CARTESIAN_POINT('Ctrl Pts',(26.1494320959692,40.1013531248915,37.6332278773558)) ;
#13978 = CARTESIAN_POINT('Ctrl Pts',(26.1124938243325,39.3682632700758,37.5996897907365)) ;
#13979 = CARTESIAN_POINT('Ctrl Pts',(26.0755555526958,38.7879703870318,37.8811625890341)) ;
#13980 = CARTESIAN_POINT('Ctrl Pts',(26.0386172810591,38.2076775039878,38.1626353873317)) ;
#13981 = CARTESIAN_POINT('Ctrl Pts',(26.0016790094224,37.7801815927156,38.759119070546)) ;
#13982 = CARTESIAN_POINT('Ctrl Pts',(25.9647407377857,37.7000880122058,39.3990814011989)) ;
#13983 = CARTESIAN_POINT('Ctrl Pts',(25.927802466149,37.6199944316959,40.0390437318518)) ;
#13984 = CARTESIAN_POINT('Ctrl Pts',(25.8908641945122,37.8873031819484,40.7224847099434)) ;
#13985 = CARTESIAN_POINT('Ctrl Pts',(25.8539259228755,38.3803295545664,41.1382872618806)) ;
#13986 = CARTESIAN_POINT('Ctrl Pts',(25.8279071792918,38.7276096573102,41.4311721073528)) ;
#13987 = CARTESIAN_POINT('Ctrl Pts',(25.801888435708,39.1868812358737,41.5912661586594)) ;
#13988 = CARTESIAN_POINT('Ctrl Pts',(25.7758696921242,39.6437968858784,41.5949974857067)) ;
#13989 = CARTESIAN_POINT('Origin',(29.6,39.642135623731,39.642135623731)) ;
#13990 = CARTESIAN_POINT('',(24.9741303078758,39.6419511053728,41.5993115726679)) ;
#13991 = CARTESIAN_POINT('',(25.0758696921242,39.6418839677207,41.5992928593099)) ;
#13992 = CARTESIAN_POINT('',(29.6,39.642135623731,41.596135623731)) ;
#13993 = CARTESIAN_POINT('Ctrl Pts',(24.9741303078758,39.6419511053728,41.5993115726679)) ;
#13994 = CARTESIAN_POINT('Ctrl Pts',(24.9747041572659,39.6319311937436,41.599325146903)) ;
#13995 = CARTESIAN_POINT('Ctrl Pts',(24.975278006656,39.6219114778643,41.5992548129635)) ;
#13996 = CARTESIAN_POINT('Ctrl Pts',(24.9758518560462,39.6118930676569,41.5990999903527)) ;
#13997 = CARTESIAN_POINT('Ctrl Pts',(25.0127901276829,38.9670152234492,41.5891341704855)) ;
#13998 = CARTESIAN_POINT('Ctrl Pts',(25.0497283993196,38.3275473055512,41.2290976426987)) ;
#13999 = CARTESIAN_POINT('Ctrl Pts',(25.0866666709563,37.9845889021496,40.6828867996612)) ;
#14000 = CARTESIAN_POINT('Ctrl Pts',(25.123604942593,37.641630498748,40.1366759566237)) ;
#14001 = CARTESIAN_POINT('Ctrl Pts',(25.1605432142298,37.5951816098427,39.4042907983354)) ;
#14002 = CARTESIAN_POINT('Ctrl Pts',(25.1974814858665,37.8663867714669,38.8191288448354)) ;
#14003 = CARTESIAN_POINT('Ctrl Pts',(25.2344197575032,38.1375919330911,38.2339668913354)) ;
#14004 = CARTESIAN_POINT('Ctrl Pts',(25.2713580291399,38.7264511452448,37.7960281426236)) ;
#14005 = CARTESIAN_POINT('Ctrl Pts',(25.3082963007766,39.3649029941181,37.7046717625188)) ;
#14006 = CARTESIAN_POINT('Ctrl Pts',(25.3452345724133,40.0033548429913,37.6133153824139)) ;
#14007 = CARTESIAN_POINT('Ctrl Pts',(25.38217284405,40.6913993285841,37.8685413709159)) ;
#14008 = CARTESIAN_POINT('Ctrl Pts',(25.4191111156868,41.1158237614022,38.3541653533783)) ;
#14009 = CARTESIAN_POINT('Ctrl Pts',(25.4560493873235,41.5402481942203,38.8397893358407)) ;
#14010 = CARTESIAN_POINT('Ctrl Pts',(25.4929876589602,41.7010525742636,39.5558113122634)) ;
#14011 = CARTESIAN_POINT('Ctrl Pts',(25.5299259305969,41.5250352795288,40.1762826359117)) ;
#14012 = CARTESIAN_POINT('Ctrl Pts',(25.5668642022336,41.3490179847941,40.7967539595599)) ;
#14013 = CARTESIAN_POINT('Ctrl Pts',(25.6038024738703,40.8361790152812,41.3216746304337)) ;
#14014 = CARTESIAN_POINT('Ctrl Pts',(25.640740745507,40.2199737307557,41.5120894377316)) ;
#14015 = CARTESIAN_POINT('Ctrl Pts',(25.6518705996299,40.0343051917945,41.5694632382416)) ;
#14016 = CARTESIAN_POINT('Ctrl Pts',(25.6630004537529,39.8392522890029,41.5964681054409)) ;
#14017 = CARTESIAN_POINT('Ctrl Pts',(25.6741303078758,39.6437755905604,41.5948983538003)) ;
#14018 = CARTESIAN_POINT('Ctrl Pts',(25.7758696921242,39.6437968858784,41.5949974857067)) ;
#14019 = CARTESIAN_POINT('Ctrl Pts',(25.7649501640713,39.8355549253086,41.596563446424)) ;
#14020 = CARTESIAN_POINT('Ctrl Pts',(25.7540306360183,40.0268980133607,41.5705891289495)) ;
#14021 = CARTESIAN_POINT('Ctrl Pts',(25.7431111079654,40.2093737712261,41.5153321335891)) ;
#14022 = CARTESIAN_POINT('Ctrl Pts',(25.7061728363287,40.8266476202843,41.3284103275775)) ;
#14023 = CARTESIAN_POINT('Ctrl Pts',(25.669234564692,41.3424513234172,40.8064025897715)) ;
#14024 = CARTESIAN_POINT('Ctrl Pts',(25.6322962930553,41.5219799101722,40.1869381010139)) ;
#14025 = CARTESIAN_POINT('Ctrl Pts',(25.5953580214185,41.7015084969271,39.5674736122563)) ;
#14026 = CARTESIAN_POINT('Ctrl Pts',(25.5584197497818,41.544761967304,38.8505523725471)) ;
#14027 = CARTESIAN_POINT('Ctrl Pts',(25.5214814781451,41.1230947222761,38.3625323926646)) ;
#14028 = CARTESIAN_POINT('Ctrl Pts',(25.4845432065084,40.7014274772481,37.8745124127821)) ;
#14029 = CARTESIAN_POINT('Ctrl Pts',(25.4476049348717,40.0148395168153,37.6153936927263)) ;
#14030 = CARTESIAN_POINT('Ctrl Pts',(25.410666663235,39.3758804888048,37.7031326625047)) ;
#14031 = CARTESIAN_POINT('Ctrl Pts',(25.3737283915982,38.7369214607943,37.7908716322831)) ;
#14032 = CARTESIAN_POINT('Ctrl Pts',(25.3367901199615,38.1455913652061,38.2254682918958)) ;
#14033 = CARTESIAN_POINT('Ctrl Pts',(25.2998518483248,37.8710764152813,38.8090848685638)) ;
#14034 = CARTESIAN_POINT('Ctrl Pts',(25.2629135766881,37.5965614653565,39.3927014452318)) ;
#14035 = CARTESIAN_POINT('Ctrl Pts',(25.2259753050514,37.6388616610951,40.1253379389552)) ;
#14036 = CARTESIAN_POINT('Ctrl Pts',(25.1890370334147,37.9787210410719,40.6734824163841)) ;
#14037 = CARTESIAN_POINT('Ctrl Pts',(25.152098761778,38.3185804210486,41.221626893813)) ;
#14038 = CARTESIAN_POINT('Ctrl Pts',(25.1151604901412,38.9559989852635,41.5852793549473)) ;
#14039 = CARTESIAN_POINT('Ctrl Pts',(25.0782222185045,39.6008100555266,41.5988973562706)) ;
#14040 = CARTESIAN_POINT('Ctrl Pts',(25.0774380430444,39.6144989747774,41.5991864575734)) ;
#14041 = CARTESIAN_POINT('Ctrl Pts',(25.0766538675843,39.6281912257218,41.599317803505)) ;
#14042 = CARTESIAN_POINT('Ctrl Pts',(25.0758696921242,39.6418839677207,41.5992928593099)) ;
#14043 = CARTESIAN_POINT('Origin',(29.6,39.642135623731,39.642135623731)) ;
#14044 = CARTESIAN_POINT('',(24.2741303078758,39.6406455788885,41.5943893719784)) ;
#14045 = CARTESIAN_POINT('',(24.3758696921242,39.6406789188743,41.5943026756172)) ;
#14046 = CARTESIAN_POINT('',(29.6,39.642135623731,41.596135623731)) ;
#14047 = CARTESIAN_POINT('Ctrl Pts',(24.2741303078758,39.6406455788885,41.5943893719784)) ;
#14048 = CARTESIAN_POINT('Ctrl Pts',(24.286407860779,39.4248694535981,41.5959340169787)) ;
#14049 = CARTESIAN_POINT('Ctrl Pts',(24.2986854136822,39.2095524239628,41.5629298688026)) ;
#14050 = CARTESIAN_POINT('Ctrl Pts',(24.3109629665853,39.00679142621,41.4933411485449)) ;
#14051 = CARTESIAN_POINT('Ctrl Pts',(24.3479012382221,38.3967642594466,41.2839763775683)) ;
#14052 = CARTESIAN_POINT('Ctrl Pts',(24.3848395098588,37.9003903593405,40.7434595224611)) ;
#14053 = CARTESIAN_POINT('Ctrl Pts',(24.4217777814955,37.7436298309467,40.1178455134642)) ;
#14054 = CARTESIAN_POINT('Ctrl Pts',(24.4587160531322,37.5868693025529,39.4922315044672)) ;
#14055 = CARTESIAN_POINT('Ctrl Pts',(24.4956543247689,37.7697221458715,38.7815203415805)) ;
#14056 = CARTESIAN_POINT('Ctrl Pts',(24.5325925964056,38.2089498028778,38.3092430746743)) ;
#14057 = CARTESIAN_POINT('Ctrl Pts',(24.5695308680423,38.6481774598841,37.8369658077682)) ;
#14058 = CARTESIAN_POINT('Ctrl Pts',(24.606469139679,39.3437799305781,37.6031224368427)) ;
#14059 = CARTESIAN_POINT('Ctrl Pts',(24.6434074113158,39.9791039676379,37.714163507846)) ;
#14060 = CARTESIAN_POINT('Ctrl Pts',(24.6803456829525,40.6144280046977,37.8252045788493)) ;
#14061 = CARTESIAN_POINT('Ctrl Pts',(24.7172839545892,41.1894736081234,38.2811300917814)) ;
#14062 = CARTESIAN_POINT('Ctrl Pts',(24.7542222262259,41.4424676167279,38.8743929198144)) ;
#14063 = CARTESIAN_POINT('Ctrl Pts',(24.7911604978626,41.6954616253324,39.4676557478475)) ;
#14064 = CARTESIAN_POINT('Ctrl Pts',(24.8280987694993,41.6264040391158,40.1982558909815)) ;
#14065 = CARTESIAN_POINT('Ctrl Pts',(24.865037041136,41.2667313607489,40.7336084065746)) ;
#14066 = CARTESIAN_POINT('Ctrl Pts',(24.9014014633826,40.9126463273361,41.2606440274954)) ;
#14067 = CARTESIAN_POINT('Ctrl Pts',(24.9377658856292,40.2769056833872,41.5984513831741)) ;
#14068 = CARTESIAN_POINT('Ctrl Pts',(24.9741303078758,39.6419511053728,41.5993115726679)) ;
#14069 = CARTESIAN_POINT('Ctrl Pts',(25.0758696921242,39.6418839677207,41.5992928593099)) ;
#14070 = CARTESIAN_POINT('Ctrl Pts',(25.0397155959476,40.2731823650047,41.5981428171641)) ;
#14071 = CARTESIAN_POINT('Ctrl Pts',(25.003561499771,40.9055245646462,41.2647771410003)) ;
#14072 = CARTESIAN_POINT('Ctrl Pts',(24.9674074035944,41.2605236498834,40.7427920084966)) ;
#14073 = CARTESIAN_POINT('Ctrl Pts',(24.9304691319577,41.6232225976656,40.2094851178871)) ;
#14074 = CARTESIAN_POINT('Ctrl Pts',(24.893530860321,41.6964169169187,39.4792877951558)) ;
#14075 = CARTESIAN_POINT('Ctrl Pts',(24.8565925886843,41.4467869748733,38.8846016104093)) ;
#14076 = CARTESIAN_POINT('Ctrl Pts',(24.8196543170475,41.1971570328278,38.2899154256628)) ;
#14077 = CARTESIAN_POINT('Ctrl Pts',(24.7827160454108,40.6247028294838,37.8307403789012)) ;
#14078 = CARTESIAN_POINT('Ctrl Pts',(24.7457777737741,39.9900178648199,37.7161028548369)) ;
#14079 = CARTESIAN_POINT('Ctrl Pts',(24.7088395021374,39.3553329001561,37.6014653307726)) ;
#14080 = CARTESIAN_POINT('Ctrl Pts',(24.6719012305007,38.6584171741724,37.8313653294056)) ;
#14081 = CARTESIAN_POINT('Ctrl Pts',(24.634962958864,38.2165217563229,38.3011474129055)) ;
#14082 = CARTESIAN_POINT('Ctrl Pts',(24.5980246872273,37.7746263384733,38.7709294964055)) ;
#14083 = CARTESIAN_POINT('Ctrl Pts',(24.5610864155906,37.587751228758,39.4805936647722)) ;
#14084 = CARTESIAN_POINT('Ctrl Pts',(24.5241481439538,37.7409660076168,40.1070854826224)) ;
#14085 = CARTESIAN_POINT('Ctrl Pts',(24.4872098723171,37.8941807864756,40.7335773004725)) ;
#14086 = CARTESIAN_POINT('Ctrl Pts',(24.4502716006804,38.3874854539086,41.276896767806)) ;
#14087 = CARTESIAN_POINT('Ctrl Pts',(24.4133333290437,38.9963170857706,41.4897131448503)) ;
#14088 = CARTESIAN_POINT('Ctrl Pts',(24.4008454500705,39.2021473912189,41.5616608847492)) ;
#14089 = CARTESIAN_POINT('Ctrl Pts',(24.3883575710974,39.4211817595164,41.5958340358532)) ;
#14090 = CARTESIAN_POINT('Ctrl Pts',(24.3758696921242,39.6406789188743,41.5943026756172)) ;
#14091 = CARTESIAN_POINT('Origin',(29.6,39.642135623731,39.642135623731)) ;
#14092 = CARTESIAN_POINT('',(23.5741303078758,39.6435118677572,41.5941173638984)) ;
#14093 = CARTESIAN_POINT('',(23.6758696921242,39.6435489601981,41.5941990304928)) ;
#14094 = CARTESIAN_POINT('',(29.6,39.642135623731,41.596135623731)) ;
#14095 = CARTESIAN_POINT('Ctrl Pts',(23.5741303078758,39.6435118677572,41.5941173638984)) ;
#14096 = CARTESIAN_POINT('Ctrl Pts',(23.598111564292,39.2218969648424,41.5913563986786)) ;
#14097 = CARTESIAN_POINT('Ctrl Pts',(23.6220928207083,38.7986808485727,41.4572211327591)) ;
#14098 = CARTESIAN_POINT('Ctrl Pts',(23.6460740771245,38.4642739167478,41.2052306124145)) ;
#14099 = CARTESIAN_POINT('Ctrl Pts',(23.6830123487612,37.9491877231577,40.8170902194008)) ;
#14100 = CARTESIAN_POINT('Ctrl Pts',(23.7199506203979,37.6448028017159,40.1493362684881)) ;
#14101 = CARTESIAN_POINT('Ctrl Pts',(23.7568888920346,37.6896817335956,39.50594476016)) ;
#14102 = CARTESIAN_POINT('Ctrl Pts',(23.7938271636714,37.7345606654753,38.8625532518319)) ;
#14103 = CARTESIAN_POINT('Ctrl Pts',(23.8307654353081,38.1287034506766,38.2435241860883)) ;
#14104 = CARTESIAN_POINT('Ctrl Pts',(23.8677037069448,38.6926877925568,37.9306529447932)) ;
#14105 = CARTESIAN_POINT('Ctrl Pts',(23.9046419785815,39.2566721344369,37.617781703498)) ;
#14106 = CARTESIAN_POINT('Ctrl Pts',(23.9415802502182,39.9904980329958,37.6110682866512)) ;
#14107 = CARTESIAN_POINT('Ctrl Pts',(23.9785185218549,40.5601121121495,37.9135687863955)) ;
#14108 = CARTESIAN_POINT('Ctrl Pts',(24.0154567934916,41.1297261913032,38.2160692861397)) ;
#14109 = CARTESIAN_POINT('Ctrl Pts',(24.0523950651284,41.5351284510516,38.8277837024749)) ;
#14110 = CARTESIAN_POINT('Ctrl Pts',(24.0893333367651,41.591771039095,39.4702464397097)) ;
#14111 = CARTESIAN_POINT('Ctrl Pts',(24.1262716084018,41.6484136271384,40.1127091769446)) ;
#14112 = CARTESIAN_POINT('Ctrl Pts',(24.1632098800385,41.3562965434769,40.785920235079)) ;
#14113 = CARTESIAN_POINT('Ctrl Pts',(24.2001481516752,40.8483977849356,41.1834194207233)) ;
#14114 = CARTESIAN_POINT('Ctrl Pts',(24.2248088704087,40.5093145556856,41.4487977175311)) ;
#14115 = CARTESIAN_POINT('Ctrl Pts',(24.2494695891422,40.0740539606037,41.5912867947634)) ;
#14116 = CARTESIAN_POINT('Ctrl Pts',(24.2741303078758,39.6406455788885,41.5943893719784)) ;
#14117 = CARTESIAN_POINT('Ctrl Pts',(24.3758696921242,39.6406789188743,41.5943026756172)) ;
#14118 = CARTESIAN_POINT('Ctrl Pts',(24.3514192994607,40.0704389883285,41.5913043794964)) ;
#14119 = CARTESIAN_POINT('Ctrl Pts',(24.3269689067971,40.5019731626006,41.4514332027079)) ;
#14120 = CARTESIAN_POINT('Ctrl Pts',(24.3025185141336,40.8396492187411,41.1902265352361)) ;
#14121 = CARTESIAN_POINT('Ctrl Pts',(24.2655802424968,41.3497911235589,40.7956102618225)) ;
#14122 = CARTESIAN_POINT('Ctrl Pts',(24.2286419708601,41.6457163369035,40.1240644282402)) ;
#14123 = CARTESIAN_POINT('Ctrl Pts',(24.1917036992234,41.5927133191848,39.4812911817476)) ;
#14124 = CARTESIAN_POINT('Ctrl Pts',(24.1547654275867,41.539710301466,38.838517935255)) ;
#14125 = CARTESIAN_POINT('Ctrl Pts',(24.11782715595,41.1377790526838,38.2245172758521)) ;
#14126 = CARTESIAN_POINT('Ctrl Pts',(24.0808888843133,40.5698873460839,37.918795546384)) ;
#14127 = CARTESIAN_POINT('Ctrl Pts',(24.0439506126766,40.0019956394839,37.613073816916)) ;
#14128 = CARTESIAN_POINT('Ctrl Pts',(24.0070123410398,39.2681434750662,37.6156310173829)) ;
#14129 = CARTESIAN_POINT('Ctrl Pts',(23.9700740694031,38.7023961857,37.9253030549788)) ;
#14130 = CARTESIAN_POINT('Ctrl Pts',(23.9331357977664,38.1366488963339,38.2349750925746)) ;
#14131 = CARTESIAN_POINT('Ctrl Pts',(23.8961975261297,37.7390064820193,38.8517619672996)) ;
#14132 = CARTESIAN_POINT('Ctrl Pts',(23.859259254493,37.6904843460513,39.494888991001)) ;
#14133 = CARTESIAN_POINT('Ctrl Pts',(23.8223209828563,37.6419622100833,40.1380160147024)) ;
#14134 = CARTESIAN_POINT('Ctrl Pts',(23.7853827112196,37.9425603524618,40.8074831873802)) ;
#14135 = CARTESIAN_POINT('Ctrl Pts',(23.7484444395829,38.4554400155153,41.1985346130523)) ;
#14136 = CARTESIAN_POINT('Ctrl Pts',(23.7242528570966,38.7913347427045,41.4546416911943)) ;
#14137 = CARTESIAN_POINT('Ctrl Pts',(23.7000612746104,39.2182810749139,41.5913309295395)) ;
#14138 = CARTESIAN_POINT('Ctrl Pts',(23.6758696921242,39.6435489601981,41.5941990304928)) ;
#14139 = CARTESIAN_POINT('Origin',(29.6,39.642135623731,39.642135623731)) ;
#14140 = CARTESIAN_POINT('',(22.8741303078758,39.6425352575914,41.5992316723864)) ;
#14141 = CARTESIAN_POINT('',(22.9758696921242,39.6424692686163,41.5992623449223)) ;
#14142 = CARTESIAN_POINT('',(29.6,39.642135623731,41.596135623731)) ;
#14143 = CARTESIAN_POINT('Ctrl Pts',(22.8741303078758,39.6425352575914,41.5992316723864)) ;
#14144 = CARTESIAN_POINT('Ctrl Pts',(22.9098152678051,39.019376320101,41.5974825577703)) ;
#14145 = CARTESIAN_POINT('Ctrl Pts',(22.9455002277344,38.3946539204701,41.2738928837315)) ;
#14146 = CARTESIAN_POINT('Ctrl Pts',(22.9811851876637,38.0377808438174,40.7631485070654)) ;
#14147 = CARTESIAN_POINT('Ctrl Pts',(23.0181234593004,37.6683738255288,40.2344659876064)) ;
#14148 = CARTESIAN_POINT('Ctrl Pts',(23.0550617309371,37.5859611047416,39.5052515727989)) ;
#14149 = CARTESIAN_POINT('Ctrl Pts',(23.0920000025738,37.8280587293757,38.9074593918063)) ;
#14150 = CARTESIAN_POINT('Ctrl Pts',(23.1289382742105,38.0701563540097,38.3096672108138)) ;
#14151 = CARTESIAN_POINT('Ctrl Pts',(23.1658765458472,38.6367643240651,37.843297263636)) ;
#14152 = CARTESIAN_POINT('Ctrl Pts',(23.2028148174839,39.2699504710714,37.7206512088624)) ;
#14153 = CARTESIAN_POINT('Ctrl Pts',(23.2397530891207,39.9031366180777,37.5980051540887)) ;
#14154 = CARTESIAN_POINT('Ctrl Pts',(23.2766913607574,40.6029009420349,37.8190829917191)) ;
#14155 = CARTESIAN_POINT('Ctrl Pts',(23.3136296323941,41.050695630241,38.2832453218724)) ;
#14156 = CARTESIAN_POINT('Ctrl Pts',(23.3505679040308,41.4984903184471,38.7474076520257)) ;
#14157 = CARTESIAN_POINT('Ctrl Pts',(23.3875061756675,41.6943153709021,39.4546544747018)) ;
#14158 = CARTESIAN_POINT('Ctrl Pts',(23.4244444473042,41.5490270002059,40.0830317824199)) ;
#14159 = CARTESIAN_POINT('Ctrl Pts',(23.4613827189409,41.4037386295096,40.7114090901379)) ;
#14160 = CARTESIAN_POINT('Ctrl Pts',(23.4983209905776,40.9173368356621,41.2609168828979)) ;
#14161 = CARTESIAN_POINT('Ctrl Pts',(23.5352592622144,40.3112422058692,41.4814073617205)) ;
#14162 = CARTESIAN_POINT('Ctrl Pts',(23.5482162774348,40.0986394771733,41.5587498675684)) ;
#14163 = CARTESIAN_POINT('Ctrl Pts',(23.5611732926553,39.8713093867623,41.5956091067727)) ;
#14164 = CARTESIAN_POINT('Ctrl Pts',(23.5741303078758,39.6435118677572,41.5941173638984)) ;
#14165 = CARTESIAN_POINT('Ctrl Pts',(23.6758696921242,39.6435489601981,41.5941990304928)) ;
#14166 = CARTESIAN_POINT('Ctrl Pts',(23.6631230029737,39.8676251463055,41.5957102499976)) ;
#14167 = CARTESIAN_POINT('Ctrl Pts',(23.6503763138232,40.0912353453651,41.5600687208437)) ;
#14168 = CARTESIAN_POINT('Ctrl Pts',(23.6376296246727,40.3008145556867,41.4851674588105)) ;
#14169 = CARTESIAN_POINT('Ctrl Pts',(23.600691353036,40.9081482490762,41.2681132002304)) ;
#14170 = CARTESIAN_POINT('Ctrl Pts',(23.5637530813993,41.3976544521269,40.721369004404)) ;
#14171 = CARTESIAN_POINT('Ctrl Pts',(23.5268148097626,41.5464993836053,40.0938246213784)) ;
#14172 = CARTESIAN_POINT('Ctrl Pts',(23.4898765381259,41.6953443150837,39.4662802383529)) ;
#14173 = CARTESIAN_POINT('Ctrl Pts',(23.4529382664891,41.5035279749898,38.7579356681281)) ;
#14174 = CARTESIAN_POINT('Ctrl Pts',(23.4159999948524,41.0583692984033,38.2912446365514)) ;
#14175 = CARTESIAN_POINT('Ctrl Pts',(23.3790617232157,40.6132106218167,37.8245536049748)) ;
#14176 = CARTESIAN_POINT('Ctrl Pts',(23.342123451579,39.9147096087375,37.5995161120464)) ;
#14177 = CARTESIAN_POINT('Ctrl Pts',(23.3051851799423,39.2808389854979,37.7185740781279)) ;
#14178 = CARTESIAN_POINT('Ctrl Pts',(23.2682469083056,38.6469683622583,37.8376320442095)) ;
#14179 = CARTESIAN_POINT('Ctrl Pts',(23.2313086366689,38.0777281288583,38.3007854693011)) ;
#14180 = CARTESIAN_POINT('Ctrl Pts',(23.1943703650321,37.8322487168373,38.8971969250653)) ;
#14181 = CARTESIAN_POINT('Ctrl Pts',(23.1574320933954,37.5867693048163,39.4936083808294)) ;
#14182 = CARTESIAN_POINT('Ctrl Pts',(23.1204938217587,37.6650507141741,40.2232778672661)) ;
#14183 = CARTESIAN_POINT('Ctrl Pts',(23.083555550122,38.031457559013,40.7540440967425)) ;
#14184 = CARTESIAN_POINT('Ctrl Pts',(23.0476602641228,38.3875185739119,41.2698236598248)) ;
#14185 = CARTESIAN_POINT('Ctrl Pts',(23.0117649781235,39.0156637705048,41.5977738151495)) ;
#14186 = CARTESIAN_POINT('Ctrl Pts',(22.9758696921242,39.6424692686163,41.5992623449223)) ;
#14187 = CARTESIAN_POINT('Origin',(29.6,39.642135623731,39.642135623731)) ;
#14188 = CARTESIAN_POINT('',(22.1741303078758,39.6404341197698,41.5952239823215)) ;
#14189 = CARTESIAN_POINT('',(22.2758696921242,39.6404509077731,41.5951215653697)) ;
#14190 = CARTESIAN_POINT('',(29.6,39.642135623731,41.596135623731)) ;
#14191 = CARTESIAN_POINT('Ctrl Pts',(22.1741303078758,39.6404341197698,41.5952239823215)) ;
#14192 = CARTESIAN_POINT('Ctrl Pts',(22.1845806996814,39.4569685731193,41.5967725865391)) ;
#14193 = CARTESIAN_POINT('Ctrl Pts',(22.195031091487,39.2738961209019,41.5730209579894)) ;
#14194 = CARTESIAN_POINT('Ctrl Pts',(22.2054814832926,39.0986059707007,41.5223482889448)) ;
#14195 = CARTESIAN_POINT('Ctrl Pts',(22.2424197549294,38.4790200926016,41.343239137007)) ;
#14196 = CARTESIAN_POINT('Ctrl Pts',(22.2793580265661,37.9566632719586,40.8277889657132)) ;
#14197 = CARTESIAN_POINT('Ctrl Pts',(22.3162962982028,37.7693236058759,40.210641817458)) ;
#14198 = CARTESIAN_POINT('Ctrl Pts',(22.3532345698395,37.5819839397931,39.5934946692027)) ;
#14199 = CARTESIAN_POINT('Ctrl Pts',(22.3901728414763,37.7296614282706,38.874650543986)) ;
#14200 = CARTESIAN_POINT('Ctrl Pts',(22.427111113113,38.1451300903487,38.3813427879068)) ;
#14201 = CARTESIAN_POINT('Ctrl Pts',(22.4640493847497,38.5605987524268,37.8880350318277)) ;
#14202 = CARTESIAN_POINT('Ctrl Pts',(22.5009876563864,39.2438585881055,37.6202636448861)) ;
#14203 = CARTESIAN_POINT('Ctrl Pts',(22.5379259280231,39.8838749852862,37.6999239394952)) ;
#14204 = CARTESIAN_POINT('Ctrl Pts',(22.5748641996598,40.5238913824668,37.7795842341044)) ;
#14205 = CARTESIAN_POINT('Ctrl Pts',(22.6118024712965,41.1206643411492,38.2066762102643)) ;
#14206 = CARTESIAN_POINT('Ctrl Pts',(22.6487407429332,41.4025299386401,38.7867783880528)) ;
#14207 = CARTESIAN_POINT('Ctrl Pts',(22.68567901457,41.6843955361311,39.3668805658413)) ;
#14208 = CARTESIAN_POINT('Ctrl Pts',(22.7226172862067,41.6513537724305,40.0999929452585)) ;
#14209 = CARTESIAN_POINT('Ctrl Pts',(22.7595555578434,41.3184459714061,40.6523869599789)) ;
#14210 = CARTESIAN_POINT('Ctrl Pts',(22.7964938294801,40.9855381703818,41.2047809746991)) ;
#14211 = CARTESIAN_POINT('Ctrl Pts',(22.8334321011168,40.3527643320338,41.5764566247226)) ;
#14212 = CARTESIAN_POINT('Ctrl Pts',(22.8703703727535,39.7081767549648,41.5982191376789)) ;
#14213 = CARTESIAN_POINT('Ctrl Pts',(22.8716236844609,39.6863059656452,41.5989575374757)) ;
#14214 = CARTESIAN_POINT('Ctrl Pts',(22.8728769961683,39.6644215759027,41.5992931040324)) ;
#14215 = CARTESIAN_POINT('Ctrl Pts',(22.8741303078758,39.6425352575914,41.5992316723864)) ;
#14216 = CARTESIAN_POINT('Ctrl Pts',(22.9758696921242,39.6424692686163,41.5992623449223)) ;
#14217 = CARTESIAN_POINT('Ctrl Pts',(22.9748267064868,39.6606819423368,41.5993055961496)) ;
#14218 = CARTESIAN_POINT('Ctrl Pts',(22.9737837208493,39.6788934849888,41.5990732253268)) ;
#14219 = CARTESIAN_POINT('Ctrl Pts',(22.9727407352119,39.6970971890957,41.5985618316083)) ;
#14220 = CARTESIAN_POINT('Ctrl Pts',(22.9358024635752,40.3417976940196,41.5804503644819)) ;
#14221 = CARTESIAN_POINT('Ctrl Pts',(22.8988641919385,40.9766664235475,41.2123644577129)) ;
#14222 = CARTESIAN_POINT('Ctrl Pts',(22.8619259203017,41.312697439253,40.6618647549232)) ;
#14223 = CARTESIAN_POINT('Ctrl Pts',(22.824987648665,41.6487284549585,40.1113650521334)) ;
#14224 = CARTESIAN_POINT('Ctrl Pts',(22.7880493770283,41.6859217568417,39.3784515533227)) ;
#14225 = CARTESIAN_POINT('Ctrl Pts',(22.7511111053916,41.407346151666,38.7967622904668)) ;
#14226 = CARTESIAN_POINT('Ctrl Pts',(22.7141728337549,41.1287705464904,38.2150730276109)) ;
#14227 = CARTESIAN_POINT('Ctrl Pts',(22.6772345621182,40.5344260342559,37.7846080007098)) ;
#14228 = CARTESIAN_POINT('Ctrl Pts',(22.6402962904815,39.8948710557536,37.7013241743502)) ;
#14229 = CARTESIAN_POINT('Ctrl Pts',(22.6033580188448,39.2553160772512,37.6180403479906)) ;
#14230 = CARTESIAN_POINT('Ctrl Pts',(22.566419747208,38.5705506324811,37.8819377221724)) ;
#14231 = CARTESIAN_POINT('Ctrl Pts',(22.5294814755713,38.1522947206771,38.3728845202077)) ;
#14232 = CARTESIAN_POINT('Ctrl Pts',(22.4925432039346,37.7340388088731,38.863831318243)) ;
#14233 = CARTESIAN_POINT('Ctrl Pts',(22.4556049322979,37.5822924300353,39.5818275401316)) ;
#14234 = CARTESIAN_POINT('Ctrl Pts',(22.4186666606612,37.7661338089679,40.2000258205355)) ;
#14235 = CARTESIAN_POINT('Ctrl Pts',(22.3817283890245,37.9499751879004,40.8182241009394)) ;
#14236 = CARTESIAN_POINT('Ctrl Pts',(22.3447901173878,38.4694043246034,41.3366244398584)) ;
#14237 = CARTESIAN_POINT('Ctrl Pts',(22.307851845751,39.0879658724486,41.519239821202)) ;
#14238 = CARTESIAN_POINT('Ctrl Pts',(22.2971911278754,39.266488306176,41.5719442649668)) ;
#14239 = CARTESIAN_POINT('Ctrl Pts',(22.2865304099998,39.45326798981,41.5966794474412)) ;
#14240 = CARTESIAN_POINT('Ctrl Pts',(22.2758696921242,39.6404509077731,41.5951215653697)) ;
#14241 = CARTESIAN_POINT('Origin',(29.6,39.642135623731,39.642135623731)) ;
#14242 = CARTESIAN_POINT('',(21.4741303078758,39.6431273922811,41.5935167596094)) ;
#14243 = CARTESIAN_POINT('',(21.5758696921242,39.643176897406,41.5935754761129)) ;
#14244 = CARTESIAN_POINT('',(29.6,39.642135623731,41.596135623731)) ;
#14245 = CARTESIAN_POINT('Ctrl Pts',(21.4741303078758,39.6431273922811,41.5935167596094)) ;
#14246 = CARTESIAN_POINT('Ctrl Pts',(21.4962844031945,39.2533349717856,41.5917134339623)) ;
#14247 = CARTESIAN_POINT('Ctrl Pts',(21.5184384985131,38.8625785317564,41.4785841605243)) ;
#14248 = CARTESIAN_POINT('Ctrl Pts',(21.5405925938318,38.5425752985296,41.2612685428463)) ;
#14249 = CARTESIAN_POINT('Ctrl Pts',(21.5775308654685,38.0090230959449,40.8989308711328)) ;
#14250 = CARTESIAN_POINT('Ctrl Pts',(21.6144691371053,37.6721649466632,40.2469549586452)) ;
#14251 = CARTESIAN_POINT('Ctrl Pts',(21.651407408742,37.6853463410244,39.6021347637736)) ;
#14252 = CARTESIAN_POINT('Ctrl Pts',(21.6883456803787,37.6985277353857,38.9573145689019)) ;
#14253 = CARTESIAN_POINT('Ctrl Pts',(21.7252839520154,38.0617486733899,38.3196500916461)) ;
#14254 = CARTESIAN_POINT('Ctrl Pts',(21.7622222236521,38.6096629521784,37.9794197241878)) ;
#14255 = CARTESIAN_POINT('Ctrl Pts',(21.7991604952888,39.1575772309668,37.6391893567295)) ;
#14256 = CARTESIAN_POINT('Ctrl Pts',(21.8360987669255,39.8901848505394,37.5963930990685)) ;
#14257 = CARTESIAN_POINT('Ctrl Pts',(21.8730370385622,40.4739871207921,37.870512846321)) ;
#14258 = CARTESIAN_POINT('Ctrl Pts',(21.909975310199,41.0577893910447,38.1446325935735)) ;
#14259 = CARTESIAN_POINT('Ctrl Pts',(21.9469135818357,41.4927863119774,38.7356683457394)) ;
#14260 = CARTESIAN_POINT('Ctrl Pts',(21.9838518534724,41.5809578536104,39.3745678231792)) ;
#14261 = CARTESIAN_POINT('Ctrl Pts',(22.0207901251091,41.6691293952435,40.013467300619)) ;
#14262 = CARTESIAN_POINT('Ctrl Pts',(22.0577283967458,41.4104755575768,40.7002305033326)) ;
#14263 = CARTESIAN_POINT('Ctrl Pts',(22.0946666683825,40.9227411709659,41.1222280383986)) ;
#14264 = CARTESIAN_POINT('Ctrl Pts',(22.1211545482136,40.5729941673948,41.4248361329995)) ;
#14265 = CARTESIAN_POINT('Ctrl Pts',(22.1476424280447,40.1054514553116,41.5912988431321)) ;
#14266 = CARTESIAN_POINT('Ctrl Pts',(22.1741303078758,39.6404341197698,41.5952239823215)) ;
#14267 = CARTESIAN_POINT('Ctrl Pts',(22.2758696921242,39.6404509077731,41.5951215653697)) ;
#14268 = CARTESIAN_POINT('Ctrl Pts',(22.2495921383631,40.1018372090838,41.5912815491187)) ;
#14269 = CARTESIAN_POINT('Ctrl Pts',(22.223314584602,40.5656734448422,41.4276925236177)) ;
#14270 = CARTESIAN_POINT('Ctrl Pts',(22.1970370308409,40.914337981394,41.1294571891952)) ;
#14271 = CARTESIAN_POINT('Ctrl Pts',(22.1600987592042,41.4044545835068,40.7102287520768)) ;
#14272 = CARTESIAN_POINT('Ctrl Pts',(22.1231604875675,41.6669938287453,40.0249414540719)) ;
#14273 = CARTESIAN_POINT('Ctrl Pts',(22.0862222159308,41.5824421877824,39.3855528493289)) ;
#14274 = CARTESIAN_POINT('Ctrl Pts',(22.049283944294,41.4978905468195,38.7461642445858)) ;
#14275 = CARTESIAN_POINT('Ctrl Pts',(22.0123456726573,41.0662480196553,38.1526743331045)) ;
#14276 = CARTESIAN_POINT('Ctrl Pts',(21.9754074010206,40.4840075992232,37.8752525310723)) ;
#14277 = CARTESIAN_POINT('Ctrl Pts',(21.9384691293839,39.9017671787911,37.5978307290401)) ;
#14278 = CARTESIAN_POINT('Ctrl Pts',(21.9015308577472,39.1689288650911,37.636477036457)) ;
#14279 = CARTESIAN_POINT('Ctrl Pts',(21.8645925861105,38.6190964543723,37.9735988043494)) ;
#14280 = CARTESIAN_POINT('Ctrl Pts',(21.8276543144738,38.0692640436535,38.3107205722417)) ;
#14281 = CARTESIAN_POINT('Ctrl Pts',(21.790716042837,37.7024375359159,38.9463178006094)) ;
#14282 = CARTESIAN_POINT('Ctrl Pts',(21.7537777712003,37.6856042889378,39.5910529552223)) ;
#14283 = CARTESIAN_POINT('Ctrl Pts',(21.7168394995636,37.6687710419596,40.2357881098352)) ;
#14284 = CARTESIAN_POINT('Ctrl Pts',(21.6799012279269,38.0019310557408,40.8896611906933)) ;
#14285 = CARTESIAN_POINT('Ctrl Pts',(21.6429629562902,38.533422666923,41.2550150036193)) ;
#14286 = CARTESIAN_POINT('Ctrl Pts',(21.6205985349015,38.8552163467658,41.476219902121)) ;
#14287 = CARTESIAN_POINT('Ctrl Pts',(21.5982341135129,39.2497133228765,41.591661008618)) ;
#14288 = CARTESIAN_POINT('Ctrl Pts',(21.5758696921242,39.643176897406,41.5935754761129)) ;
#14289 = CARTESIAN_POINT('Origin',(29.6,39.642135623731,39.642135623731)) ;
#14290 = CARTESIAN_POINT('',(20.7741303078758,39.6430525564623,41.598752263752)) ;
#14291 = CARTESIAN_POINT('',(20.8758696921242,39.6430106825472,41.5988377495572)) ;
#14292 = CARTESIAN_POINT('',(29.6,39.642135623731,41.596135623731)) ;
#14293 = CARTESIAN_POINT('Ctrl Pts',(20.7741303078758,39.6430525564623,41.598752263752)) ;
#14294 = CARTESIAN_POINT('Ctrl Pts',(20.8079881067075,39.0514242059577,41.5952420385212)) ;
#14295 = CARTESIAN_POINT('Ctrl Pts',(20.8418459055392,38.4568801100053,41.3080512591221)) ;
#14296 = CARTESIAN_POINT('Ctrl Pts',(20.875703704371,38.0948628415535,40.8407051836536)) ;
#14297 = CARTESIAN_POINT('Ctrl Pts',(20.9126419760077,37.6999082768545,40.3308387162615)) ;
#14298 = CARTESIAN_POINT('Ctrl Pts',(20.9495802476444,37.5817171822124,39.6065436368026)) ;
#14299 = CARTESIAN_POINT('Ctrl Pts',(20.9865185192811,37.7941178194275,38.9975639952763)) ;
#14300 = CARTESIAN_POINT('Ctrl Pts',(21.0234567909178,38.0065184566426,38.38858435375)) ;
#14301 = CARTESIAN_POINT('Ctrl Pts',(21.0603950625546,38.5495108257149,37.8949201501563)) ;
#14302 = CARTESIAN_POINT('Ctrl Pts',(21.0973333341913,39.1759005105809,37.7412833052911)) ;
#14303 = CARTESIAN_POINT('Ctrl Pts',(21.134271605828,39.8022901954467,37.5876464604258)) ;
#14304 = CARTESIAN_POINT('Ctrl Pts',(21.1712098774647,40.5120771961061,37.7740369742889)) ;
#14305 = CARTESIAN_POINT('Ctrl Pts',(21.2081481491014,40.9821574581571,38.2156132098312)) ;
#14306 = CARTESIAN_POINT('Ctrl Pts',(21.2450864207381,41.4522377202081,38.6571894453736)) ;
#14307 = CARTESIAN_POINT('Ctrl Pts',(21.2820246923748,41.6826112436507,39.3539514025952)) ;
#14308 = CARTESIAN_POINT('Ctrl Pts',(21.3189629640115,41.5684038796714,39.9887143339762)) ;
#14309 = CARTESIAN_POINT('Ctrl Pts',(21.3559012356483,41.4541965156921,40.6234772653574)) ;
#14310 = CARTESIAN_POINT('Ctrl Pts',(21.392839507285,40.9954082642909,41.196241170898)) ;
#14311 = CARTESIAN_POINT('Ctrl Pts',(21.4297777789217,40.4008910106465,41.4462734081986)) ;
#14312 = CARTESIAN_POINT('Ctrl Pts',(21.4445619552397,40.1629413851623,41.5463463276301)) ;
#14313 = CARTESIAN_POINT('Ctrl Pts',(21.4593461315577,39.9032490442437,41.5947201797419)) ;
#14314 = CARTESIAN_POINT('Ctrl Pts',(21.4741303078758,39.6431273922811,41.5935167596094)) ;
#14315 = CARTESIAN_POINT('Ctrl Pts',(21.5758696921242,39.643176897406,41.5935754761129)) ;
#14316 = CARTESIAN_POINT('Ctrl Pts',(21.5612958418762,39.8995787561265,41.5948230452806)) ;
#14317 = CARTESIAN_POINT('Ctrl Pts',(21.5467219916281,40.1555417786995,41.5478612892325)) ;
#14318 = CARTESIAN_POINT('Ctrl Pts',(21.53214814138,40.3906611063697,41.4505420266541)) ;
#14319 = CARTESIAN_POINT('Ctrl Pts',(21.4952098697433,40.9865847260513,41.2038806917688)) ;
#14320 = CARTESIAN_POINT('Ctrl Pts',(21.4582715981066,41.4486087568314,40.6337234770042)) ;
#14321 = CARTESIAN_POINT('Ctrl Pts',(21.4213333264699,41.566409737262,39.9996179837209)) ;
#14322 = CARTESIAN_POINT('Ctrl Pts',(21.3843950548332,41.6842107176926,39.3655124904376)) ;
#14323 = CARTESIAN_POINT('Ctrl Pts',(21.3474567831965,41.4577886477738,38.6674587186358)) ;
#14324 = CARTESIAN_POINT('Ctrl Pts',(21.3105185115598,40.990216052329,38.2232263199088)) ;
#14325 = CARTESIAN_POINT('Ctrl Pts',(21.2735802399231,40.5226434568841,37.7789939211818)) ;
#14326 = CARTESIAN_POINT('Ctrl Pts',(21.2366419682863,39.8139203359133,37.5885828955297)) ;
#14327 = CARTESIAN_POINT('Ctrl Pts',(21.1997036966496,39.1866721101622,37.7386714115382)) ;
#14328 = CARTESIAN_POINT('Ctrl Pts',(21.1627654250129,38.5594238844111,37.8887599275467)) ;
#14329 = CARTESIAN_POINT('Ctrl Pts',(21.1258271533762,38.0136505538797,38.3793479852159)) ;
#14330 = CARTESIAN_POINT('Ctrl Pts',(21.0888888817395,37.797801167441,38.9871113914114)) ;
#14331 = CARTESIAN_POINT('Ctrl Pts',(21.0519506101028,37.5819517810022,39.5948747976069)) ;
#14332 = CARTESIAN_POINT('Ctrl Pts',(21.0150123384661,37.6960263386562,40.3198135523287)) ;
#14333 = CARTESIAN_POINT('Ctrl Pts',(20.9780740668294,38.0880931290849,40.831915760622)) ;
#14334 = CARTESIAN_POINT('Ctrl Pts',(20.9440059419277,38.4496958731846,41.3042270307907)) ;
#14335 = CARTESIAN_POINT('Ctrl Pts',(20.9099378170259,39.0477685794782,41.595492055224)) ;
#14336 = CARTESIAN_POINT('Ctrl Pts',(20.8758696921242,39.6430106825472,41.5988377495572)) ;
#14337 = CARTESIAN_POINT('Origin',(29.6,39.642135623731,39.642135623731)) ;
#14338 = CARTESIAN_POINT('',(20.1,39.642135623731,41.596135623731)) ;
#14339 = CARTESIAN_POINT('',(20.1758696921242,39.6403856614379,41.5960667040991)) ;
#14340 = CARTESIAN_POINT('',(29.6,39.642135623731,41.596135623731)) ;
#14341 = CARTESIAN_POINT('',(20.1,39.1924719723276,41.5436925123374)) ;
#14342 = CARTESIAN_POINT('Origin',(20.1,39.642135623731,39.642135623731)) ;
#14343 = CARTESIAN_POINT('Ctrl Pts',(20.1,39.1924719723275,41.5436925123374)) ;
#14344 = CARTESIAN_POINT('Ctrl Pts',(20.1369382716367,38.561997188093,41.3946033132209)) ;
#14345 = CARTESIAN_POINT('Ctrl Pts',(20.1738765432734,38.0168810177416,40.9084697851729)) ;
#14346 = CARTESIAN_POINT('Ctrl Pts',(20.2108148149101,37.7999421624532,40.3022386179921)) ;
#14347 = CARTESIAN_POINT('Ctrl Pts',(20.2477530865469,37.5830033071648,39.6960074508112)) ;
#14348 = CARTESIAN_POINT('Ctrl Pts',(20.2846913581836,37.6942417669393,38.9696786444975)) ;
#14349 = CARTESIAN_POINT('Ctrl Pts',(20.3216296298203,38.0847160955708,38.4562506191992)) ;
#14350 = CARTESIAN_POINT('Ctrl Pts',(20.358567901457,38.4751904242022,37.9428225939008)) ;
#14351 = CARTESIAN_POINT('Ctrl Pts',(20.3955061730937,39.1449006216906,37.6422953496178)) ;
#14352 = CARTESIAN_POINT('Ctrl Pts',(20.4324444447304,39.7881721301733,37.6905138623107)) ;
#14353 = CARTESIAN_POINT('Ctrl Pts',(20.4693827163671,40.4314436386561,37.7387323750036)) ;
#14354 = CARTESIAN_POINT('Ctrl Pts',(20.5063209880039,41.0482764581332,38.1356966446725)) ;
#14355 = CARTESIAN_POINT('Ctrl Pts',(20.5432592596406,41.3582757099971,38.701169032257)) ;
#14356 = CARTESIAN_POINT('Ctrl Pts',(20.5801975312773,41.6682749618611,39.2666414198415)) ;
#14357 = CARTESIAN_POINT('Ctrl Pts',(20.617135802914,41.6714406461119,40.0006219253415)) ;
#14358 = CARTESIAN_POINT('Ctrl Pts',(20.6540740745507,41.3661313458041,40.5687529999006)) ;
#14359 = CARTESIAN_POINT('Ctrl Pts',(20.6910123461874,41.0608220454964,41.1368840744597)) ;
#14360 = CARTESIAN_POINT('Ctrl Pts',(20.7279506178241,40.4470377606301,41.5391657180777)) ;
#14361 = CARTESIAN_POINT('Ctrl Pts',(20.7648888894608,39.8042866008192,41.5925876122242)) ;
#14362 = CARTESIAN_POINT('Ctrl Pts',(20.7679693622658,39.750684269675,41.597042739246)) ;
#14363 = CARTESIAN_POINT('Ctrl Pts',(20.7710498350708,39.6968804811139,41.599071633402)) ;
#14364 = CARTESIAN_POINT('Ctrl Pts',(20.7741303078758,39.6430525564623,41.598752263752)) ;
#14365 = CARTESIAN_POINT('Ctrl Pts',(20.8758696921242,39.6430106825472,41.5988377495572)) ;
#14366 = CARTESIAN_POINT('Ctrl Pts',(20.8729995453892,39.6931582085291,41.5991196151924)) ;
#14367 = CARTESIAN_POINT('Ctrl Pts',(20.8701293986542,39.7432856440115,41.5973579435593)) ;
#14368 = CARTESIAN_POINT('Ctrl Pts',(20.8672592519192,39.7932498983189,41.5934888294942)) ;
#14369 = CARTESIAN_POINT('Ctrl Pts',(20.8303209802825,40.4362808539208,41.5436940282085)) ;
#14370 = CARTESIAN_POINT('Ctrl Pts',(20.7933827086458,41.0522837419213,41.1448387637723)) ;
#14371 = CARTESIAN_POINT('Ctrl Pts',(20.7564444370091,41.3608307362133,40.5784740403519)) ;
#14372 = CARTESIAN_POINT('Ctrl Pts',(20.7195061653724,41.6693777305054,40.0121093169316)) ;
#14373 = CARTESIAN_POINT('Ctrl Pts',(20.6825678937356,41.6704688310889,39.2782351345271)) ;
#14374 = CARTESIAN_POINT('Ctrl Pts',(20.6456296220989,41.36362737304,38.7109598395018)) ;
#14375 = CARTESIAN_POINT('Ctrl Pts',(20.6086913504622,41.0567859149911,38.1436845444765)) ;
#14376 = CARTESIAN_POINT('Ctrl Pts',(20.5717530788255,40.4420118983097,37.7430081368304)) ;
#14377 = CARTESIAN_POINT('Ctrl Pts',(20.5348148071888,39.7991237067178,37.6912612551126)) ;
#14378 = CARTESIAN_POINT('Ctrl Pts',(20.4978765355521,39.156235515126,37.6395143733948)) ;
#14379 = CARTESIAN_POINT('Ctrl Pts',(20.4609382639154,38.4852331486237,37.9366970176053)) ;
#14380 = CARTESIAN_POINT('Ctrl Pts',(20.4239999922786,38.0916512795126,38.447656902979)) ;
#14381 = CARTESIAN_POINT('Ctrl Pts',(20.3870617206419,37.6980694104016,38.9586167883527)) ;
#14382 = CARTESIAN_POINT('Ctrl Pts',(20.3501234490052,37.5819080386817,39.6833539148898)) ;
#14383 = CARTESIAN_POINT('Ctrl Pts',(20.3131851773685,37.7958866514344,40.2916891358699)) ;
#14384 = CARTESIAN_POINT('Ctrl Pts',(20.2762469057318,38.0098652641872,40.90002435685)) ;
#14385 = CARTESIAN_POINT('Ctrl Pts',(20.2393086340951,38.5539838614125,41.3919576722732)) ;
#14386 = CARTESIAN_POINT('Ctrl Pts',(20.2023703624584,39.1808671084928,41.5440782600819)) ;
#14387 = CARTESIAN_POINT('Ctrl Pts',(20.1935368056803,39.3307823186778,41.5804569478217)) ;
#14388 = CARTESIAN_POINT('Ctrl Pts',(20.1847032489023,39.4854308170824,41.59740183643)) ;
#14389 = CARTESIAN_POINT('Ctrl Pts',(20.1758696921242,39.6403856614379,41.5960667040991)) ;
#14390 = CARTESIAN_POINT('Origin',(30.6940562256037,39.642135623731,39.642135623731)) ;
#14391 = CARTESIAN_POINT('',(20.5440562256037,39.6428655566193,41.1997186245255)) ;
#14392 = CARTESIAN_POINT('',(20.4059437743963,39.6407425498585,41.1975807596125)) ;
#14393 = CARTESIAN_POINT('',(30.6940562256037,39.6421356237311,41.197635623731)) ;
#14394 = CARTESIAN_POINT('',(20.1,38.4771632437029,38.6076638930866)) ;
#14395 = CARTESIAN_POINT('Ctrl Pts',(20.5440562256037,39.6428655566193,41.1997186245255)) ;
#14396 = CARTESIAN_POINT('Ctrl Pts',(20.5409757527987,39.6857157801584,41.1999728617264)) ;
#14397 = CARTESIAN_POINT('Ctrl Pts',(20.500957008357,40.242137908518,41.1789906663339)) ;
#14398 = CARTESIAN_POINT('Ctrl Pts',(20.4239999922786,41.260102964655,40.5118040569248)) ;
#14399 = CARTESIAN_POINT('Ctrl Pts',(20.3131851773685,41.2525427468677,38.758927890642)) ;
#14400 = CARTESIAN_POINT('Ctrl Pts',(20.2051851799423,39.8168546376957,37.8349872964746)) ;
#14401 = CARTESIAN_POINT('Ctrl Pts',(20.1341234541528,38.7943081205531,38.2545323388419)) ;
#14402 = CARTESIAN_POINT('Ctrl Pts',(20.1,38.4771632437029,38.6076638930866)) ;
#14403 = CARTESIAN_POINT('',(20.1,40.2413475545766,38.2066826248723)) ;
#14404 = CARTESIAN_POINT('Origin',(20.1,39.642135623731,39.642135623731)) ;
#14405 = CARTESIAN_POINT('Ctrl Pts',(20.4059437743963,39.6407425498585,41.1975807596125)) ;
#14406 = CARTESIAN_POINT('Ctrl Pts',(20.3778390595376,40.0332014593976,41.1941992288133)) ;
#14407 = CARTESIAN_POINT('Ctrl Pts',(20.3127960730423,40.9471855575388,40.8454705034782)) ;
#14408 = CARTESIAN_POINT('Ctrl Pts',(20.2108148149101,41.4478477610965,39.3100962723047)) ;
#14409 = CARTESIAN_POINT('Ctrl Pts',(20.1369382716367,40.7172822611094,38.4053556254406)) ;
#14410 = CARTESIAN_POINT('Ctrl Pts',(20.1,40.2413475545766,38.2066826248723)) ;
#14411 = CARTESIAN_POINT('Origin',(30.6940562256037,39.642135623731,39.642135623731)) ;
#14412 = CARTESIAN_POINT('',(21.2440562256037,39.6429251303736,41.1955508524203)) ;
#14413 = CARTESIAN_POINT('',(21.1059437743963,39.642832222497,41.1997866763014)) ;
#14414 = CARTESIAN_POINT('',(30.6940562256037,39.6421356237311,41.197635623731)) ;
#14415 = CARTESIAN_POINT('Ctrl Pts',(21.2440562256037,39.6429251303736,41.1955508524203)) ;
#14416 = CARTESIAN_POINT('Ctrl Pts',(21.2292720492857,39.8499974075629,41.1965088462873)) ;
#14417 = CARTESIAN_POINT('Ctrl Pts',(21.177549601331,40.5732442315414,41.061786987415)) ;
#14418 = CARTESIAN_POINT('Ctrl Pts',(21.0888888817395,41.4498663517249,39.9673877570378)) ;
#14419 = CARTESIAN_POINT('Ctrl Pts',(20.9780740668294,40.8996933490919,38.3033961125266)) ;
#14420 = CARTESIAN_POINT('Ctrl Pts',(20.8672592519192,39.2045955811405,37.8582623699771)) ;
#14421 = CARTESIAN_POINT('Ctrl Pts',(20.7564444370091,37.907833098911,39.0372204078837)) ;
#14422 = CARTESIAN_POINT('Ctrl Pts',(20.6487100949039,38.1822480719097,40.7188819177846)) ;
#14423 = CARTESIAN_POINT('Ctrl Pts',(20.5779140244354,39.1718942673614,41.1969242768559)) ;
#14424 = CARTESIAN_POINT('Ctrl Pts',(20.5440562256037,39.6428655566193,41.1997186245255)) ;
#14425 = CARTESIAN_POINT('Ctrl Pts',(21.1059437743963,39.642832222497,41.1997866763014)) ;
#14426 = CARTESIAN_POINT('Ctrl Pts',(21.1030736276613,39.6827526302068,41.2000110580801)) ;
#14427 = CARTESIAN_POINT('Ctrl Pts',(21.0632652092896,40.2362196732324,41.1805600891616)) ;
#14428 = CARTESIAN_POINT('Ctrl Pts',(20.9865185192811,41.2550721079325,40.520864063088)) ;
#14429 = CARTESIAN_POINT('Ctrl Pts',(20.875703704371,41.257677850447,38.7682418152935)) ;
#14430 = CARTESIAN_POINT('Ctrl Pts',(20.7648888894608,39.7894880096876,37.8113551948838)) ;
#14431 = CARTESIAN_POINT('Ctrl Pts',(20.6540740745507,38.1870148554998,38.5210802763619)) ;
#14432 = CARTESIAN_POINT('Ctrl Pts',(20.5432592596406,37.9096008119324,40.25188160747)) ;
#14433 = CARTESIAN_POINT('Ctrl Pts',(20.4605491595891,38.8794875060849,41.1287484880954)) ;
#14434 = CARTESIAN_POINT('Ctrl Pts',(20.4147773311743,39.5173892947945,41.1986436042086)) ;
#14435 = CARTESIAN_POINT('Ctrl Pts',(20.4059437743963,39.6407425498585,41.1975807596125)) ;
#14436 = CARTESIAN_POINT('Origin',(30.6940562256037,39.642135623731,39.642135623731)) ;
#14437 = CARTESIAN_POINT('',(21.9440562256037,39.6407811255675,41.1969099030491)) ;
#14438 = CARTESIAN_POINT('',(21.8059437743963,39.6429645393921,41.1955975942428)) ;
#14439 = CARTESIAN_POINT('',(30.6940562256037,39.6421356237311,41.197635623731)) ;
#14440 = CARTESIAN_POINT('Ctrl Pts',(21.9440562256037,39.6407811255675,41.1969099030491)) ;
#14441 = CARTESIAN_POINT('Ctrl Pts',(21.9175683457726,40.0109625306009,41.1937852592368)) ;
#14442 = CARTESIAN_POINT('Ctrl Pts',(21.8541421943048,40.9021886596065,40.876475390125)) ;
#14443 = CARTESIAN_POINT('Ctrl Pts',(21.7537777712003,41.4616468090319,39.3910334034537)) ;
#14444 = CARTESIAN_POINT('Ctrl Pts',(21.6429629562902,40.4227966905405,37.9795347660523)) ;
#14445 = CARTESIAN_POINT('Ctrl Pts',(21.53214814138,38.6731992203584,38.0817398511981)) ;
#14446 = CARTESIAN_POINT('Ctrl Pts',(21.4213333264699,37.8057629321309,39.6045961885133)) ;
#14447 = CARTESIAN_POINT('Ctrl Pts',(21.3253026878778,38.5029121757861,40.9539015719257)) ;
#14448 = CARTESIAN_POINT('Ctrl Pts',(21.2662103209224,39.3326272234746,41.1941152981501)) ;
#14449 = CARTESIAN_POINT('Ctrl Pts',(21.2440562256037,39.6429251303736,41.1955508524203)) ;
#14450 = CARTESIAN_POINT('Ctrl Pts',(21.8059437743963,39.6429645393921,41.1955975942428)) ;
#14451 = CARTESIAN_POINT('Ctrl Pts',(21.7913699241482,39.8470756403336,41.1965907333627)) ;
#14452 = CARTESIAN_POINT('Ctrl Pts',(21.7398578022635,40.56728344443,41.0644535876924)) ;
#14453 = CARTESIAN_POINT('Ctrl Pts',(21.6514074087419,41.4479940364311,39.977619430384)) ;
#14454 = CARTESIAN_POINT('Ctrl Pts',(21.5405925938318,40.9072578085518,38.3105427025879)) ;
#14455 = CARTESIAN_POINT('Ctrl Pts',(21.4297777789217,39.2147007747696,37.8558072618482)) ;
#14456 = CARTESIAN_POINT('Ctrl Pts',(21.3189629640115,37.9112968612974,39.0274189154373)) ;
#14457 = CARTESIAN_POINT('Ctrl Pts',(21.2110182958364,38.1766711691164,40.7138608723637)) ;
#14458 = CARTESIAN_POINT('Ctrl Pts',(21.140011899298,39.168984171666,41.1971233049938)) ;
#14459 = CARTESIAN_POINT('Ctrl Pts',(21.1059437743963,39.642832222497,41.1997866763014)) ;
#14460 = CARTESIAN_POINT('Origin',(30.6940562256037,39.642135623731,39.642135623731)) ;
#14461 = CARTESIAN_POINT('',(22.6440562256037,39.6424537560083,41.2001002622589)) ;
#14462 = CARTESIAN_POINT('',(22.5059437743963,39.6407944898148,41.1968283730754)) ;
#14463 = CARTESIAN_POINT('',(30.6940562256037,39.6421356237311,41.197635623731)) ;
#14464 = CARTESIAN_POINT('Ctrl Pts',(22.6440562256037,39.6424537560083,41.2001002622589)) ;
#14465 = CARTESIAN_POINT('Ctrl Pts',(22.6428029138963,39.6598765646743,41.200149165496)) ;
#14466 = CARTESIAN_POINT('Ctrl Pts',(22.6046113305522,40.1907469072132,41.1920090101158)) ;
#14467 = CARTESIAN_POINT('Ctrl Pts',(22.5294814755713,41.2152893427001,40.5902182080807)) ;
#14468 = CARTESIAN_POINT('Ctrl Pts',(22.4186666606612,41.2941989590302,38.8394152814942)) ;
#14469 = CARTESIAN_POINT('Ctrl Pts',(22.307851845751,39.8689988506925,37.8194435789608)) ;
#14470 = CARTESIAN_POINT('Ctrl Pts',(22.1970370308409,38.2372526771025,38.4589293400473)) ;
#14471 = CARTESIAN_POINT('Ctrl Pts',(22.0862222159307,37.884572533817,40.1756571344811)) ;
#14472 = CARTESIAN_POINT('Ctrl Pts',(22.0018952808517,38.8338703266282,41.1124032256132)) ;
#14473 = CARTESIAN_POINT('Ctrl Pts',(21.9545066174093,39.4947316589273,41.1981426839398)) ;
#14474 = CARTESIAN_POINT('Ctrl Pts',(21.9440562256037,39.6407811255675,41.1969099030491)) ;
#14475 = CARTESIAN_POINT('Ctrl Pts',(22.5059437743963,39.6407944898148,41.1968283730754)) ;
#14476 = CARTESIAN_POINT('Ctrl Pts',(22.4796662206352,40.0080853760424,41.1937714921755)) ;
#14477 = CARTESIAN_POINT('Ctrl Pts',(22.4164503952374,40.8963676775261,40.8804858433475)) ;
#14478 = CARTESIAN_POINT('Ctrl Pts',(22.3162962982028,41.4630397864066,39.4013424185359)) ;
#14479 = CARTESIAN_POINT('Ctrl Pts',(22.2054814832927,40.432200557639,37.9839828116129)) ;
#14480 = CARTESIAN_POINT('Ctrl Pts',(22.0946666683825,38.682052148795,38.0762770764856)) ;
#14481 = CARTESIAN_POINT('Ctrl Pts',(21.9838518534724,37.806005117906,39.594196455287)) ;
#14482 = CARTESIAN_POINT('Ctrl Pts',(21.8876108888103,38.4970109681013,40.9503919933712)) ;
#14483 = CARTESIAN_POINT('Ctrl Pts',(21.8283081957849,39.3297441759424,41.1940735644637)) ;
#14484 = CARTESIAN_POINT('Ctrl Pts',(21.8059437743963,39.6429645393921,41.1955975942428)) ;
#14485 = CARTESIAN_POINT('Origin',(30.6940562256037,39.642135623731,39.642135623731)) ;
#14486 = CARTESIAN_POINT('',(23.3440562256037,39.6432311956772,41.1960289690894)) ;
#14487 = CARTESIAN_POINT('',(23.2059437743963,39.6424012248667,41.2001246794184)) ;
#14488 = CARTESIAN_POINT('',(30.6940562256037,39.6421356237311,41.197635623731)) ;
#14489 = CARTESIAN_POINT('Ctrl Pts',(23.3440562256037,39.6432311956772,41.1960289690894)) ;
#14490 = CARTESIAN_POINT('Ctrl Pts',(23.3310992103832,39.8245715440971,41.1972164849753)) ;
#14491 = CARTESIAN_POINT('Ctrl Pts',(23.2812039235261,40.5214498349615,41.0842248278971)) ;
#14492 = CARTESIAN_POINT('Ctrl Pts',(23.1943703650321,41.4316808979472,40.0558999560533)) ;
#14493 = CARTESIAN_POINT('Ctrl Pts',(23.083555550122,40.9640157969843,38.366868585522)) ;
#14494 = CARTESIAN_POINT('Ctrl Pts',(22.9727407352119,39.2928539659985,37.8388953361349)) ;
#14495 = CARTESIAN_POINT('Ctrl Pts',(22.8619259203017,37.9396932227727,38.9526698287169)) ;
#14496 = CARTESIAN_POINT('Ctrl Pts',(22.752364417099,38.1342834924026,40.6744674861658)) ;
#14497 = CARTESIAN_POINT('Ctrl Pts',(22.679741185533,39.1463822476838,41.1987078631876)) ;
#14498 = CARTESIAN_POINT('Ctrl Pts',(22.6440562256037,39.6424537560083,41.2001002622589)) ;
#14499 = CARTESIAN_POINT('Ctrl Pts',(23.2059437743963,39.6424012248667,41.2001246794184)) ;
#14500 = CARTESIAN_POINT('Ctrl Pts',(23.2049007887588,39.6568995943509,41.2001591099629)) ;
#14501 = CARTESIAN_POINT('Ctrl Pts',(23.1669195314847,40.184837931591,41.1934228620692)) ;
#14502 = CARTESIAN_POINT('Ctrl Pts',(23.0920000025738,41.2098945632884,40.5991127594935)) ;
#14503 = CARTESIAN_POINT('Ctrl Pts',(22.9811851876637,41.2987187921716,38.848784795215)) ;
#14504 = CARTESIAN_POINT('Ctrl Pts',(22.8703703727535,39.8793182464488,37.8207576467842)) ;
#14505 = CARTESIAN_POINT('Ctrl Pts',(22.7595555578434,38.2439764102052,38.4509915754534)) ;
#14506 = CARTESIAN_POINT('Ctrl Pts',(22.6487407429332,37.8815790320852,40.1656944257316)) ;
#14507 = CARTESIAN_POINT('Ctrl Pts',(22.5642034817842,38.8279106834674,41.1101517427012)) ;
#14508 = CARTESIAN_POINT('Ctrl Pts',(22.5166044922719,39.4917857749265,41.1980685396886)) ;
#14509 = CARTESIAN_POINT('Ctrl Pts',(22.5059437743963,39.6407944898148,41.1968283730754)) ;
#14510 = CARTESIAN_POINT('Origin',(30.6940562256037,39.642135623731,39.642135623731)) ;
#14511 = CARTESIAN_POINT('',(24.0440562256037,39.6409494595793,41.196245503669)) ;
#14512 = CARTESIAN_POINT('',(23.9059437743963,39.6432607234622,41.1960939805468)) ;
#14513 = CARTESIAN_POINT('',(30.6940562256037,39.6421356237311,41.197635623731)) ;
#14514 = CARTESIAN_POINT('Ctrl Pts',(24.0440562256037,39.6409494595793,41.196245503669)) ;
#14515 = CARTESIAN_POINT('Ctrl Pts',(24.0193955068702,39.9859682608884,41.1937756680201)) ;
#14516 = CARTESIAN_POINT('Ctrl Pts',(23.9577965164999,40.8514594910534,40.9104441463242)) ;
#14517 = CARTESIAN_POINT('Ctrl Pts',(23.859259254493,41.4717945581916,39.4808241401565)) ;
#14518 = CARTESIAN_POINT('Ctrl Pts',(23.7484444395829,40.5036217613051,38.0199411699272)) ;
#14519 = CARTESIAN_POINT('Ctrl Pts',(23.6376296246727,38.7511148239329,38.0359740049913)) ;
#14520 = CARTESIAN_POINT('Ctrl Pts',(23.5268148097626,37.8098316575348,39.5143256607193)) ;
#14521 = CARTESIAN_POINT('Ctrl Pts',(23.4289570100729,38.4517613530902,40.9225790274919)) ;
#14522 = CARTESIAN_POINT('Ctrl Pts',(23.36803748202,39.3076007036178,41.1938310768686)) ;
#14523 = CARTESIAN_POINT('Ctrl Pts',(23.3440562256037,39.6432311956772,41.1960289690894)) ;
#14524 = CARTESIAN_POINT('Ctrl Pts',(23.9059437743963,39.6432607234622,41.1960939805468)) ;
#14525 = CARTESIAN_POINT('Ctrl Pts',(23.8931970852458,39.821638669977,41.1972970009867)) ;
#14526 = CARTESIAN_POINT('Ctrl Pts',(23.8435121244586,40.5154871172593,41.0867035675646)) ;
#14527 = CARTESIAN_POINT('Ctrl Pts',(23.7568888920346,41.4293088255812,40.0660286263046)) ;
#14528 = CARTESIAN_POINT('Ctrl Pts',(23.6460740771245,40.9712172436731,38.3743756391225)) ;
#14529 = CARTESIAN_POINT('Ctrl Pts',(23.5352592622143,39.3030724240549,37.8369460276841)) ;
#14530 = CARTESIAN_POINT('Ctrl Pts',(23.4244444473042,37.9436253671659,38.9430388926739)) ;
#14531 = CARTESIAN_POINT('Ctrl Pts',(23.3146726180315,38.1288157471692,40.669218461723)) ;
#14532 = CARTESIAN_POINT('Ctrl Pts',(23.2418390603956,39.1434268378081,41.198939721352)) ;
#14533 = CARTESIAN_POINT('Ctrl Pts',(23.2059437743963,39.6424012248667,41.2001246794184)) ;
#14534 = CARTESIAN_POINT('Origin',(30.6940562256037,39.642135623731,39.642135623731)) ;
#14535 = CARTESIAN_POINT('',(24.7440562256037,39.641988736164,41.2001638676263)) ;
#14536 = CARTESIAN_POINT('',(24.6059437743963,39.6409760001874,41.1961764882187)) ;
#14537 = CARTESIAN_POINT('',(30.6940562256037,39.6421356237311,41.197635623731)) ;
#14538 = CARTESIAN_POINT('Ctrl Pts',(24.7440562256037,39.641988736164,41.2001638676263)) ;
#14539 = CARTESIAN_POINT('Ctrl Pts',(24.7076918033571,40.1474502745986,41.1994791057237)) ;
#14540 = CARTESIAN_POINT('Ctrl Pts',(24.6343891094738,41.1676111809988,40.6574060741533)) ;
#14541 = CARTESIAN_POINT('Ctrl Pts',(24.5241481439538,41.3316789557939,38.9216381981518)) ;
#14542 = CARTESIAN_POINT('Ctrl Pts',(24.4133333290437,39.9583676413693,37.8328068746627)) ;
#14543 = CARTESIAN_POINT('Ctrl Pts',(24.3025185141336,38.2971450571862,38.3912664910517)) ;
#14544 = CARTESIAN_POINT('Ctrl Pts',(24.1917036992234,37.8604599019426,40.0885713229918)) ;
#14545 = CARTESIAN_POINT('Ctrl Pts',(24.1055496030468,38.7820838555419,41.092156082151)) ;
#14546 = CARTESIAN_POINT('Ctrl Pts',(24.0563337785069,39.4691788542113,41.1974751327877)) ;
#14547 = CARTESIAN_POINT('Ctrl Pts',(24.0440562256037,39.6409494595793,41.196245503669)) ;
#14548 = CARTESIAN_POINT('Ctrl Pts',(24.6059437743963,39.6409760001874,41.1961764882187)) ;
#14549 = CARTESIAN_POINT('Ctrl Pts',(24.5814933817327,39.9830905283532,41.1937896665114)) ;
#14550 = CARTESIAN_POINT('Ctrl Pts',(24.5201047174324,40.8455982589183,40.9142290234479)) ;
#14551 = CARTESIAN_POINT('Ctrl Pts',(24.4217777814955,41.4726788523376,39.4911892118972)) ;
#14552 = CARTESIAN_POINT('Ctrl Pts',(24.3109629665853,40.5127954478126,38.0248462860509)) ;
#14553 = CARTESIAN_POINT('Ctrl Pts',(24.2001481516752,38.7602257828917,38.0309533361934)) ;
#14554 = CARTESIAN_POINT('Ctrl Pts',(24.0893333367651,37.8105848789005,39.5039502404432)) ;
#14555 = CARTESIAN_POINT('Ctrl Pts',(23.9912652110054,38.445891019574,40.9188512189262)) ;
#14556 = CARTESIAN_POINT('Ctrl Pts',(23.9301353568825,39.304722240576,41.193810801922)) ;
#14557 = CARTESIAN_POINT('Ctrl Pts',(23.9059437743963,39.6432607234622,41.1960939805468)) ;
#14558 = CARTESIAN_POINT('Origin',(30.6940562256037,39.642135623731,39.642135623731)) ;
#14559 = CARTESIAN_POINT('',(25.4440562256037,39.6434411346846,41.1966506834151)) ;
#14560 = CARTESIAN_POINT('',(25.3059437743963,39.6419352906073,41.2001489706823)) ;
#14561 = CARTESIAN_POINT('',(30.6940562256037,39.6421356237311,41.197635623731)) ;
#14562 = CARTESIAN_POINT('Ctrl Pts',(25.4440562256037,39.6434411346846,41.1966506834151)) ;
#14563 = CARTESIAN_POINT('Ctrl Pts',(25.4329263714808,39.799052191198,41.1979002989099)) ;
#14564 = CARTESIAN_POINT('Ctrl Pts',(25.3848582457212,40.4696553434449,41.10505600482)) ;
#14565 = CARTESIAN_POINT('Ctrl Pts',(25.2998518483248,41.4091655775236,40.1434123472918)) ;
#14566 = CARTESIAN_POINT('Ctrl Pts',(25.1890370334147,41.0251360793291,38.4334243467918)) ;
#14567 = CARTESIAN_POINT('Ctrl Pts',(25.0782222185045,39.3819633096162,37.8238992314671)) ;
#14568 = CARTESIAN_POINT('Ctrl Pts',(24.9674074035944,37.9756626373976,38.8697749586234)) ;
#14569 = CARTESIAN_POINT('Ctrl Pts',(24.8565925886842,38.0865908564746,40.6188411516388)) ;
#14570 = CARTESIAN_POINT('Ctrl Pts',(24.7821421960207,39.1126080506474,41.196514648151)) ;
#14571 = CARTESIAN_POINT('Ctrl Pts',(24.7446300749939,39.634012291671,41.2001746735233)) ;
#14572 = CARTESIAN_POINT('Ctrl Pts',(24.7440562256037,39.641988736164,41.2001638676263)) ;
#14573 = CARTESIAN_POINT('Ctrl Pts',(25.3059437743963,39.6419352906073,41.2001489706824)) ;
#14574 = CARTESIAN_POINT('Ctrl Pts',(25.2697896782197,40.1444862921299,41.1992334688615)) ;
#14575 = CARTESIAN_POINT('Ctrl Pts',(25.1966973104064,41.16216841065,40.6627197145167)) ;
#14576 = CARTESIAN_POINT('Ctrl Pts',(25.0866666709563,41.3357325096837,38.9312186673045)) ;
#14577 = CARTESIAN_POINT('Ctrl Pts',(24.9758518560461,39.9686099201725,37.8346268783008)) ;
#14578 = CARTESIAN_POINT('Ctrl Pts',(24.8650370411361,38.304251048472,38.3836690193557)) ;
#14579 = CARTESIAN_POINT('Ctrl Pts',(24.7542222262259,37.8579600047224,40.0784734419163)) ;
#14580 = CARTESIAN_POINT('Ctrl Pts',(24.6678578039793,38.7761213015138,41.0897245806797)) ;
#14581 = CARTESIAN_POINT('Ctrl Pts',(24.6184316533695,39.4662432308008,41.1973955418764)) ;
#14582 = CARTESIAN_POINT('Ctrl Pts',(24.6059437743963,39.6409760001874,41.1961764882187)) ;
#14583 = CARTESIAN_POINT('Origin',(30.6940562256037,39.642135623731,39.642135623731)) ;
#14584 = CARTESIAN_POINT('',(26.1440562256037,39.6412226456937,41.1957096458694)) ;
#14585 = CARTESIAN_POINT('',(26.0059437743963,39.6434580870219,41.1967295982976)) ;
#14586 = CARTESIAN_POINT('',(30.6940562256037,39.6421356237311,41.197635623731)) ;
#14587 = CARTESIAN_POINT('Ctrl Pts',(26.1440562256037,39.6412226456937,41.1957096458694)) ;
#14588 = CARTESIAN_POINT('Ctrl Pts',(26.1212226679677,39.9609555622393,41.1939883019333)) ;
#14589 = CARTESIAN_POINT('Ctrl Pts',(26.0614508386951,40.800410911607,40.9424746399457)) ;
#14590 = CARTESIAN_POINT('Ctrl Pts',(25.9647407377856,41.477513974956,39.571005327472)) ;
#14591 = CARTESIAN_POINT('Ctrl Pts',(25.8539259228755,40.5823617185973,38.064273747103)) ;
#14592 = CARTESIAN_POINT('Ctrl Pts',(25.7431111079654,38.8311870681316,37.9940956814497)) ;
#14593 = CARTESIAN_POINT('Ctrl Pts',(25.6322962930552,37.8183349635443,39.4243642686637)) ;
#14594 = CARTESIAN_POINT('Ctrl Pts',(25.532611332268,38.4009054869355,40.8893367037083)) ;
#14595 = CARTESIAN_POINT('Ctrl Pts',(25.4698646431175,39.2826030615248,41.1937530175458)) ;
#14596 = CARTESIAN_POINT('Ctrl Pts',(25.4440562256037,39.6434411346846,41.1966506834151)) ;
#14597 = CARTESIAN_POINT('Ctrl Pts',(26.0059437743963,39.6434580870219,41.1967295982976)) ;
#14598 = CARTESIAN_POINT('Ctrl Pts',(25.9950242463433,39.7961088702019,41.1979761959925)) ;
#14599 = CARTESIAN_POINT('Ctrl Pts',(25.9471664466537,40.4636946757718,41.1073531908352)) ;
#14600 = CARTESIAN_POINT('Ctrl Pts',(25.8623703753273,41.4062982291994,40.1534120973844)) ;
#14601 = CARTESIAN_POINT('Ctrl Pts',(25.7515555604172,41.0319596004962,38.4412764960012)) ;
#14602 = CARTESIAN_POINT('Ctrl Pts',(25.640740745507,39.392265272267,37.822454844445)) ;
#14603 = CARTESIAN_POINT('Ctrl Pts',(25.5299259305969,37.9800636903518,38.8603490676194)) ;
#14604 = CARTESIAN_POINT('Ctrl Pts',(25.4191111156867,38.0810840912803,40.6100154944158)) ;
#14605 = CARTESIAN_POINT('Ctrl Pts',(25.3444503969532,39.1067023870668,41.1951390511897)) ;
#14606 = CARTESIAN_POINT('Ctrl Pts',(25.3067279498564,39.631035055101,41.2001688277425)) ;
#14607 = CARTESIAN_POINT('Ctrl Pts',(25.3059437743963,39.6419352906073,41.2001489706824)) ;
#14608 = CARTESIAN_POINT('Origin',(30.6940562256037,39.642135623731,39.642135623731)) ;
#14609 = CARTESIAN_POINT('',(26.8440562256037,39.6415425595799,41.1998999830041)) ;
#14610 = CARTESIAN_POINT('',(26.7059437743963,39.6412597076922,41.1956580485042)) ;
#14611 = CARTESIAN_POINT('',(30.6940562256037,39.6421356237311,41.197635623731)) ;
#14612 = CARTESIAN_POINT('Ctrl Pts',(26.8440562256037,39.6415425595799,41.1998999830041)) ;
#14613 = CARTESIAN_POINT('Ctrl Pts',(26.8095189644547,40.1218241840523,41.1975493661777)) ;
#14614 = CARTESIAN_POINT('Ctrl Pts',(26.7380434316689,41.1199631784081,40.7026026237249)) ;
#14615 = CARTESIAN_POINT('Ctrl Pts',(26.6296296272465,41.3650697227584,39.0056049473486)) ;
#14616 = CARTESIAN_POINT('Ctrl Pts',(26.5188148123364,40.0469710495945,37.8505493184767)) ;
#14617 = CARTESIAN_POINT('Ctrl Pts',(26.4079999974262,38.3602927420783,38.3266311433769)) ;
#14618 = CARTESIAN_POINT('Ctrl Pts',(26.2971851825161,37.8406594871401,40.0004049924068)) ;
#14619 = CARTESIAN_POINT('Ctrl Pts',(26.2092039252419,38.7302854054079,41.0703220356036)) ;
#14620 = CARTESIAN_POINT('Ctrl Pts',(26.1581609396045,39.4437176656815,41.1967729520918)) ;
#14621 = CARTESIAN_POINT('Ctrl Pts',(26.1440562256037,39.6412226456937,41.1957096458694)) ;
#14622 = CARTESIAN_POINT('Ctrl Pts',(26.7059437743963,39.6412597076922,41.1956580485042)) ;
#14623 = CARTESIAN_POINT('Ctrl Pts',(26.6833205428303,39.9580738929038,41.194025130763)) ;
#14624 = CARTESIAN_POINT('Ctrl Pts',(26.6237590396275,40.7945171726604,40.9460395382985)) ;
#14625 = CARTESIAN_POINT('Ctrl Pts',(26.5272592647882,41.4778874257816,39.5814013470451)) ;
#14626 = CARTESIAN_POINT('Ctrl Pts',(26.416444449878,40.5912830608963,38.0696241059467)) ;
#14627 = CARTESIAN_POINT('Ctrl Pts',(26.3056296349679,38.8405339270694,37.9895291820938)) ;
#14628 = CARTESIAN_POINT('Ctrl Pts',(26.1948148200577,37.8195975555487,39.4140384490947)) ;
#14629 = CARTESIAN_POINT('Ctrl Pts',(26.0949195332006,38.3950733473823,40.8853847393576)) ;
#14630 = CARTESIAN_POINT('Ctrl Pts',(26.0319625179801,39.2797261046359,41.1937592404563)) ;
#14631 = CARTESIAN_POINT('Ctrl Pts',(26.0059437743963,39.6434580870219,41.1967295982976)) ;
#14632 = CARTESIAN_POINT('Origin',(30.6940562256037,39.642135623731,39.642135623731)) ;
#14633 = CARTESIAN_POINT('',(27.5440562256037,39.6435335091576,41.197371464458)) ;
#14634 = CARTESIAN_POINT('',(27.4059437743963,39.6414949228124,41.1998520948235)) ;
#14635 = CARTESIAN_POINT('',(30.6940562256037,39.6421356237311,41.197635623731)) ;
#14636 = CARTESIAN_POINT('Ctrl Pts',(27.5440562256037,39.6435335091576,41.197371464458)) ;
#14637 = CARTESIAN_POINT('Ctrl Pts',(27.5347535325783,39.7734451527461,41.1985318984516)) ;
#14638 = CARTESIAN_POINT('Ctrl Pts',(27.4885125679163,40.4178911838916,41.1243328333579)) ;
#14639 = CARTESIAN_POINT('Ctrl Pts',(27.4053333316175,41.3823734685628,40.2297114846548)) ;
#14640 = CARTESIAN_POINT('Ctrl Pts',(27.2945185167073,41.0829090703606,38.5029055750713)) ;
#14641 = CARTESIAN_POINT('Ctrl Pts',(27.1837037017972,39.4717023486403,37.8133038337068)) ;
#14642 = CARTESIAN_POINT('Ctrl Pts',(27.0728888868871,38.0156654467869,38.7887494467938)) ;
#14643 = CARTESIAN_POINT('Ctrl Pts',(26.9620740719769,38.0404371457719,40.5411546443971)) ;
#14644 = CARTESIAN_POINT('Ctrl Pts',(26.8857965182158,39.0612544298047,41.1839889943965)) ;
#14645 = CARTESIAN_POINT('Ctrl Pts',(26.8464572360914,39.6081536578824,41.2000633965309)) ;
#14646 = CARTESIAN_POINT('Ctrl Pts',(26.8440562256037,39.6415425595799,41.1998999830041)) ;
#14647 = CARTESIAN_POINT('Ctrl Pts',(27.4059437743963,39.6414949228124,41.1998520948236)) ;
#14648 = CARTESIAN_POINT('Ctrl Pts',(27.3716168393172,40.1188907313755,41.1973562034564)) ;
#14649 = CARTESIAN_POINT('Ctrl Pts',(27.3003516326014,41.1144275745993,40.7076660016292)) ;
#14650 = CARTESIAN_POINT('Ctrl Pts',(27.192148154249,41.3686471870141,39.0153731842676)) ;
#14651 = CARTESIAN_POINT('Ctrl Pts',(27.0813333393388,40.0571114221001,37.8528708534111)) ;
#14652 = CARTESIAN_POINT('Ctrl Pts',(26.9705185244287,38.367763791755,38.3193923515952)) ;
#14653 = CARTESIAN_POINT('Ctrl Pts',(26.8597037095185,37.8386592473608,39.9901963817902)) ;
#14654 = CARTESIAN_POINT('Ctrl Pts',(26.7715121261745,38.724323513277,41.0677045090039)) ;
#14655 = CARTESIAN_POINT('Ctrl Pts',(26.720258814467,39.4407928670888,41.1966912909403)) ;
#14656 = CARTESIAN_POINT('Ctrl Pts',(26.7059437743963,39.6412597076922,41.1956580485042)) ;
#14657 = CARTESIAN_POINT('Origin',(30.6940562256037,39.642135623731,39.642135623731)) ;
#14658 = CARTESIAN_POINT('',(28.2440562256037,39.6415737394006,41.1953392395473)) ;
#14659 = CARTESIAN_POINT('',(28.1059437743963,39.6435359003472,41.1974583899176)) ;
#14660 = CARTESIAN_POINT('',(30.6940562256037,39.6421356237311,41.197635623731)) ;
#14661 = CARTESIAN_POINT('Ctrl Pts',(28.2440562256037,39.6415737394006,41.1953392395473)) ;
#14662 = CARTESIAN_POINT('Ctrl Pts',(28.2230498290653,39.9358973857211,41.1943802817051)) ;
#14663 = CARTESIAN_POINT('Ctrl Pts',(28.1651051608901,40.7491092810725,40.9726167632119)) ;
#14664 = CARTESIAN_POINT('Ctrl Pts',(28.0702222210783,41.4787901727068,39.6613583328092)) ;
#14665 = CARTESIAN_POINT('Ctrl Pts',(27.9594074061682,40.6588265422981,38.1124254201628)) ;
#14666 = CARTESIAN_POINT('Ctrl Pts',(27.848592591258,38.9132218087539,37.956206051659)) ;
#14667 = CARTESIAN_POINT('Ctrl Pts',(27.7377777763479,37.8312525732956,39.3349299949331)) ;
#14668 = CARTESIAN_POINT('Ctrl Pts',(27.6362656544631,38.3504124819495,40.8541260832666)) ;
#14669 = CARTESIAN_POINT('Ctrl Pts',(27.571691804215,39.257604033775,41.1939241546557)) ;
#14670 = CARTESIAN_POINT('Ctrl Pts',(27.5440562256037,39.6435335091576,41.197371464458)) ;
#14671 = CARTESIAN_POINT('Ctrl Pts',(28.1059437743963,39.6435359003471,41.1974583899176)) ;
#14672 = CARTESIAN_POINT('Ctrl Pts',(28.0968514074409,39.7704922710606,41.1986001215001)) ;
#14673 = CARTESIAN_POINT('Ctrl Pts',(28.0508207688488,40.4119358388835,41.126454460646)) ;
#14674 = CARTESIAN_POINT('Ctrl Pts',(27.96785185862,41.3790176807763,40.2395580544964)) ;
#14675 = CARTESIAN_POINT('Ctrl Pts',(27.8570370437098,41.0893382026773,38.5110838439939)) ;
#14676 = CARTESIAN_POINT('Ctrl Pts',(27.7462222287997,39.4820628559708,37.812367849582)) ;
#14677 = CARTESIAN_POINT('Ctrl Pts',(27.6354074138896,38.02052476931,38.7795514216669)) ;
#14678 = CARTESIAN_POINT('Ctrl Pts',(27.5245925989794,38.0353711001173,40.5320688312148)) ;
#14679 = CARTESIAN_POINT('Ctrl Pts',(27.4481047191483,39.0553359645197,41.1824628553531)) ;
#14680 = CARTESIAN_POINT('Ctrl Pts',(27.408555110954,39.6051782191946,41.2000419635769)) ;
#14681 = CARTESIAN_POINT('Ctrl Pts',(27.4059437743963,39.6414949228124,41.1998520948236)) ;
#14682 = CARTESIAN_POINT('Origin',(30.6940562256037,39.642135623731,39.642135623731)) ;
#14683 = CARTESIAN_POINT('',(28.9440562256037,39.6410873345839,41.199362363652)) ;
#14684 = CARTESIAN_POINT('',(28.8059437743963,39.6416116368869,41.195305032435)) ;
#14685 = CARTESIAN_POINT('',(30.6940562256037,39.6421356237311,41.197635623731)) ;
#14686 = CARTESIAN_POINT('Ctrl Pts',(28.9440562256037,39.6410873345839,41.199362363652)) ;
#14687 = CARTESIAN_POINT('Ctrl Pts',(28.9113461255522,40.0963330616707,41.1960267055326)) ;
#14688 = CARTESIAN_POINT('Ctrl Pts',(28.8416977538641,41.0716738723266,40.7456795001595)) ;
#14689 = CARTESIAN_POINT('Ctrl Pts',(28.7351111105392,41.3942255244127,39.0910907111602)) ;
#14690 = CARTESIAN_POINT('Ctrl Pts',(28.624296295629,40.1346271265577,37.8726387777184)) ;
#14691 = CARTESIAN_POINT('Ctrl Pts',(28.5134814807189,38.4265266238107,38.2651743224326)) ;
#14692 = CARTESIAN_POINT('Ctrl Pts',(28.4026666658087,37.8252273599387,39.911374245203)) ;
#14693 = CARTESIAN_POINT('Ctrl Pts',(28.312858247437,38.6785065574203,41.0468480488814)) ;
#14694 = CARTESIAN_POINT('Ctrl Pts',(28.259988100702,39.4183499435878,41.1960665416592)) ;
#14695 = CARTESIAN_POINT('Ctrl Pts',(28.2440562256037,39.6415737394006,41.1953392395473)) ;
#14696 = CARTESIAN_POINT('Ctrl Pts',(28.8059437743963,39.6416116368869,41.195305032435)) ;
#14697 = CARTESIAN_POINT('Ctrl Pts',(28.7851477039278,39.9330056123089,41.1944331137349)) ;
#14698 = CARTESIAN_POINT('Ctrl Pts',(28.7274133618227,40.7432003839351,40.9759731746722)) ;
#14699 = CARTESIAN_POINT('Ctrl Pts',(28.6327407480808,41.4786453053513,39.671756482491)) ;
#14700 = CARTESIAN_POINT('Ctrl Pts',(28.5219259331707,40.6674772372708,38.1182099023464)) ;
#14701 = CARTESIAN_POINT('Ctrl Pts',(28.4111111182605,38.9227802986979,37.9521038579512)) ;
#14702 = CARTESIAN_POINT('Ctrl Pts',(28.3002963033504,37.8330223043396,39.324679226451)) ;
#14703 = CARTESIAN_POINT('Ctrl Pts',(28.1985738553956,38.3446264340712,40.8499443789831)) ;
#14704 = CARTESIAN_POINT('Ctrl Pts',(28.1337896790776,39.2547246023744,41.1939617702834)) ;
#14705 = CARTESIAN_POINT('Ctrl Pts',(28.1059437743963,39.6435359003471,41.1974583899176)) ;
#14706 = CARTESIAN_POINT('Origin',(20.1,39.642135623731,39.642135623731)) ;
#14707 = CARTESIAN_POINT('Ctrl Pts',(20.1,38.4771632437029,38.6076638930866)) ;
#14708 = CARTESIAN_POINT('Ctrl Pts',(20.1,38.4471842989757,38.633695702627)) ;
#14709 = CARTESIAN_POINT('Ctrl Pts',(20.1,38.4183276248831,38.6608956116623)) ;
#14710 = CARTESIAN_POINT('Ctrl Pts',(20.1,38.3906795143262,38.6892240882464)) ;
#14711 = CARTESIAN_POINT('Ctrl Pts',(20.1,38.3492091017984,38.7317150066697)) ;
#14712 = CARTESIAN_POINT('Ctrl Pts',(20.1,38.3104558584504,38.7767427355807)) ;
#14713 = CARTESIAN_POINT('Ctrl Pts',(20.1,38.2744245066081,38.8239788897696)) ;
#14714 = CARTESIAN_POINT('Ctrl Pts',(20.1,38.2522070410619,38.8531054025028)) ;
#14715 = CARTESIAN_POINT('Ctrl Pts',(20.1,38.231024980398,38.883072537858)) ;
#14716 = CARTESIAN_POINT('Ctrl Pts',(20.1,38.2108850074198,38.9138110407869)) ;
#14717 = CARTESIAN_POINT('Ctrl Pts',(20.1,38.2038364321758,38.9245688829656)) ;
#14718 = CARTESIAN_POINT('Ctrl Pts',(20.1,38.1969169630732,38.9354192430819)) ;
#14719 = CARTESIAN_POINT('Ctrl Pts',(20.1,38.1901324830045,38.9463496455857)) ;
#14720 = CARTESIAN_POINT('Ctrl Pts',(20.1,38.1572723307046,38.9992902817637)) ;
#14721 = CARTESIAN_POINT('Ctrl Pts',(20.1,38.1275364351092,39.0541653253696)) ;
#14722 = CARTESIAN_POINT('Ctrl Pts',(20.1,38.1009316604637,39.1106156981426)) ;
#14723 = CARTESIAN_POINT('Ctrl Pts',(20.1,38.0804217583057,39.1541338875573)) ;
#14724 = CARTESIAN_POINT('Ctrl Pts',(20.1,38.0617732267877,39.1985894369993)) ;
#14725 = CARTESIAN_POINT('Ctrl Pts',(20.1,38.0450033095947,39.2438334856589)) ;
#14726 = CARTESIAN_POINT('Ctrl Pts',(20.1,38.0383575665427,39.2617632296501)) ;
#14727 = CARTESIAN_POINT('Ctrl Pts',(20.1,38.0320069970726,39.2798169309718)) ;
#14728 = CARTESIAN_POINT('Ctrl Pts',(20.1,38.0259532717025,39.2979857743449)) ;
#14729 = CARTESIAN_POINT('Ctrl Pts',(20.1,38.0220625131859,39.3096629776816)) ;
#14730 = CARTESIAN_POINT('Ctrl Pts',(20.1,38.0182944593548,39.3213878357419)) ;
#14731 = CARTESIAN_POINT('Ctrl Pts',(20.1,38.014653688814,39.3331439108972)) ;
#14732 = CARTESIAN_POINT('Ctrl Pts',(20.1,37.9955205478867,39.3949249652588)) ;
#14733 = CARTESIAN_POINT('Ctrl Pts',(20.1,37.9798674930171,39.4576596257358)) ;
#14734 = CARTESIAN_POINT('Ctrl Pts',(20.1,37.9677029541813,39.5209827002554)) ;
#14735 = CARTESIAN_POINT('Ctrl Pts',(20.1,37.9552821571085,39.5856397389857)) ;
#14736 = CARTESIAN_POINT('Ctrl Pts',(20.1,37.9464978419906,39.6509111700541)) ;
#14737 = CARTESIAN_POINT('Ctrl Pts',(20.1,37.9414013169079,39.7164413416117)) ;
#14738 = CARTESIAN_POINT('Ctrl Pts',(20.1,37.9380042773892,39.7601198438917)) ;
#14739 = CARTESIAN_POINT('Ctrl Pts',(20.1,37.9362465210122,39.8039139704257)) ;
#14740 = CARTESIAN_POINT('Ctrl Pts',(20.1,37.9361552286675,39.84772306421)) ;
#14741 = CARTESIAN_POINT('Ctrl Pts',(20.1,37.93610984702,39.8695006717415)) ;
#14742 = CARTESIAN_POINT('Ctrl Pts',(20.1,37.9364764227937,39.891282016996)) ;
#14743 = CARTESIAN_POINT('Ctrl Pts',(20.1,37.9372592574947,39.9130548757857)) ;
#14744 = CARTESIAN_POINT('Ctrl Pts',(20.1,37.9377989933606,39.9280664647964)) ;
#14745 = CARTESIAN_POINT('Ctrl Pts',(20.1,37.9385366154168,39.9430740212226)) ;
#14746 = CARTESIAN_POINT('Ctrl Pts',(20.1,37.9394737196895,39.9580735415047)) ;
#14747 = CARTESIAN_POINT('Ctrl Pts',(20.1,37.9401376118804,39.9686999623553)) ;
#14748 = CARTESIAN_POINT('Ctrl Pts',(20.1,37.9409010314124,39.9793127680792)) ;
#14749 = CARTESIAN_POINT('Ctrl Pts',(20.1,37.9417640229791,39.9899103038919)) ;
#14750 = CARTESIAN_POINT('Ctrl Pts',(20.1,37.9472618141605,40.0574231756069)) ;
#14751 = CARTESIAN_POINT('Ctrl Pts',(20.1,37.9567969806614,40.124316733486)) ;
#14752 = CARTESIAN_POINT('Ctrl Pts',(20.1,37.9704106721731,40.1902188479243)) ;
#14753 = CARTESIAN_POINT('Ctrl Pts',(20.1,37.9736714320761,40.2060037635811)) ;
#14754 = CARTESIAN_POINT('Ctrl Pts',(20.1,37.9771663964514,40.2217318853767)) ;
#14755 = CARTESIAN_POINT('Ctrl Pts',(20.1,37.9808965550334,40.237398231313)) ;
#14756 = CARTESIAN_POINT('Ctrl Pts',(20.1,37.9959250015805,40.3005164171257)) ;
#14757 = CARTESIAN_POINT('Ctrl Pts',(20.1,38.0147669309706,40.3626320365636)) ;
#14758 = CARTESIAN_POINT('Ctrl Pts',(20.1,38.0371591550646,40.4235632338164)) ;
#14759 = CARTESIAN_POINT('Ctrl Pts',(20.1,38.0493406366329,40.4567101089616)) ;
#14760 = CARTESIAN_POINT('Ctrl Pts',(20.1,38.0625737285448,40.4895064459427)) ;
#14761 = CARTESIAN_POINT('Ctrl Pts',(20.1,38.0768223050403,40.5219221617345)) ;
#14762 = CARTESIAN_POINT('Ctrl Pts',(20.1,38.0891447183764,40.5499558287257)) ;
#14763 = CARTESIAN_POINT('Ctrl Pts',(20.1,38.1022266974373,40.5777048279095)) ;
#14764 = CARTESIAN_POINT('Ctrl Pts',(20.1,38.116047303518,40.6051489944802)) ;
#14765 = CARTESIAN_POINT('Ctrl Pts',(20.1,38.1207119187167,40.6144117197005)) ;
#14766 = CARTESIAN_POINT('Ctrl Pts',(20.1,38.1254594051322,40.6236370495224)) ;
#14767 = CARTESIAN_POINT('Ctrl Pts',(20.1,38.1302848214216,40.6328168606391)) ;
#14768 = CARTESIAN_POINT('Ctrl Pts',(20.1,38.1618484692572,40.6928631463702)) ;
#14769 = CARTESIAN_POINT('Ctrl Pts',(20.1,38.1967886424964,40.7510552902723)) ;
#14770 = CARTESIAN_POINT('Ctrl Pts',(20.1,38.2347975138951,40.8072008920799)) ;
#14771 = CARTESIAN_POINT('Ctrl Pts',(20.1,38.2736045218223,40.8645254780053)) ;
#14772 = CARTESIAN_POINT('Ctrl Pts',(20.1,38.3156108209451,40.9197174906792)) ;
#14773 = CARTESIAN_POINT('Ctrl Pts',(20.1,38.3605432443238,40.9725628487746)) ;
#14774 = CARTESIAN_POINT('Ctrl Pts',(20.1,38.4058108269567,41.0258023901674)) ;
#14775 = CARTESIAN_POINT('Ctrl Pts',(20.1,38.454048885018,41.0766610251022)) ;
#14776 = CARTESIAN_POINT('Ctrl Pts',(20.1,38.5050257934815,41.1248975541876)) ;
#14777 = CARTESIAN_POINT('Ctrl Pts',(20.1,38.5181105797675,41.1372789380982)) ;
#14778 = CARTESIAN_POINT('Ctrl Pts',(20.1,38.5313760345214,41.1494874120446)) ;
#14779 = CARTESIAN_POINT('Ctrl Pts',(20.1,38.5448186744254,41.1615185503207)) ;
#14780 = CARTESIAN_POINT('Ctrl Pts',(20.1,38.5539017265004,41.1696478654154)) ;
#14781 = CARTESIAN_POINT('Ctrl Pts',(20.1,38.5630662700531,41.1776966072414)) ;
#14782 = CARTESIAN_POINT('Ctrl Pts',(20.1,38.5722987266649,41.1856529081345)) ;
#14783 = CARTESIAN_POINT('Ctrl Pts',(20.1,38.6269868720595,41.2327817881649)) ;
#14784 = CARTESIAN_POINT('Ctrl Pts',(20.1,38.6841537809393,41.2767594894807)) ;
#14785 = CARTESIAN_POINT('Ctrl Pts',(20.1,38.7435015175629,41.3173659232921)) ;
#14786 = CARTESIAN_POINT('Ctrl Pts',(20.1,38.8029893136318,41.3580681874572)) ;
#14787 = CARTESIAN_POINT('Ctrl Pts',(20.1,38.8646688888385,41.3953841416024)) ;
#14788 = CARTESIAN_POINT('Ctrl Pts',(20.1,38.9282849740291,41.4290653215661)) ;
#14789 = CARTESIAN_POINT('Ctrl Pts',(20.1,38.9905426948541,41.4620273231251)) ;
#14790 = CARTESIAN_POINT('Ctrl Pts',(20.1,39.0546558560331,41.4915088253113)) ;
#14791 = CARTESIAN_POINT('Ctrl Pts',(20.1,39.1204174970525,41.5172396967087)) ;
#14792 = CARTESIAN_POINT('Ctrl Pts',(20.1,39.1442223983483,41.5265539541447)) ;
#14793 = CARTESIAN_POINT('Ctrl Pts',(20.1,39.1682435659401,41.5353763365805)) ;
#14794 = CARTESIAN_POINT('Ctrl Pts',(20.1,39.1924719723276,41.5436925123374)) ;
#14795 = CARTESIAN_POINT('',(20.1,40.8748717950665,41.1621520113221)) ;
#14796 = CARTESIAN_POINT('Origin',(20.1,39.642135623731,39.642135623731)) ;
#14797 = CARTESIAN_POINT('Ctrl Pts',(20.1,40.8749138146613,41.1621829179885)) ;
#14798 = CARTESIAN_POINT('Ctrl Pts',(20.1,40.910118556837,41.1277159927359)) ;
#14799 = CARTESIAN_POINT('Ctrl Pts',(20.1,40.9438718690891,41.091885062196)) ;
#14800 = CARTESIAN_POINT('Ctrl Pts',(20.1,40.9760625743085,41.0547102740498)) ;
#14801 = CARTESIAN_POINT('Ctrl Pts',(20.1,41.0231100315383,41.0003784648081)) ;
#14802 = CARTESIAN_POINT('Ctrl Pts',(20.1,41.0668218688122,40.943176514036)) ;
#14803 = CARTESIAN_POINT('Ctrl Pts',(20.1,41.10711615432,40.8834720571114)) ;
#14804 = CARTESIAN_POINT('Ctrl Pts',(20.1,41.1273251615833,40.8535281633699)) ;
#14805 = CARTESIAN_POINT('Ctrl Pts',(20.1,41.1466737625269,40.822954478093)) ;
#14806 = CARTESIAN_POINT('Ctrl Pts',(20.1,41.1651469177346,40.7917962001638)) ;
#14807 = CARTESIAN_POINT('Ctrl Pts',(20.1,41.1726171516231,40.7791963155703)) ;
#14808 = CARTESIAN_POINT('Ctrl Pts',(20.1,41.1799453503731,40.7664987577444)) ;
#14809 = CARTESIAN_POINT('Ctrl Pts',(20.1,41.1871266089476,40.7537132305828)) ;
#14810 = CARTESIAN_POINT('Ctrl Pts',(20.1,41.2220665911135,40.6915060162942)) ;
#14811 = CARTESIAN_POINT('Ctrl Pts',(20.1,41.25346410526,40.6273417786838)) ;
#14812 = CARTESIAN_POINT('Ctrl Pts',(20.1,41.2812451501811,40.5615844124439)) ;
#14813 = CARTESIAN_POINT('Ctrl Pts',(20.1,41.3017750166453,40.512990489797)) ;
#14814 = CARTESIAN_POINT('Ctrl Pts',(20.1,41.3203288925696,40.4635259999673)) ;
#14815 = CARTESIAN_POINT('Ctrl Pts',(20.1,41.3368587922048,40.413335412753)) ;
#14816 = CARTESIAN_POINT('Ctrl Pts',(20.1,41.345542673033,40.3869680973014)) ;
#14817 = CARTESIAN_POINT('Ctrl Pts',(20.1,41.3536677048483,40.3604003853126)) ;
#14818 = CARTESIAN_POINT('Ctrl Pts',(20.1,41.3612251844057,40.333653400688)) ;
#14819 = CARTESIAN_POINT('Ctrl Pts',(20.1,41.3646856421227,40.3214063534219)) ;
#14820 = CARTESIAN_POINT('Ctrl Pts',(20.1,41.3680270907377,40.3091217232312)) ;
#14821 = CARTESIAN_POINT('Ctrl Pts',(20.1,41.3712486093269,40.2968015581035)) ;
#14822 = CARTESIAN_POINT('Ctrl Pts',(20.1,41.3743356306514,40.2849957555236)) ;
#14823 = CARTESIAN_POINT('Ctrl Pts',(20.1,41.3773099420866,40.2731672101754)) ;
#14824 = CARTESIAN_POINT('Ctrl Pts',(20.1,41.3801712759402,40.2613177481751)) ;
#14825 = CARTESIAN_POINT('Ctrl Pts',(20.1,41.3965090601543,40.193659109539)) ;
#14826 = CARTESIAN_POINT('Ctrl Pts',(20.1,41.4091677309796,40.1253186782015)) ;
#14827 = CARTESIAN_POINT('Ctrl Pts',(20.1,41.4180675225836,40.056631121656)) ;
#14828 = CARTESIAN_POINT('Ctrl Pts',(20.1,41.4267500723293,39.9896202125065)) ;
#14829 = CARTESIAN_POINT('Ctrl Pts',(20.1,41.4318548797362,39.922277949119)) ;
#14830 = CARTESIAN_POINT('Ctrl Pts',(20.1,41.4332596199026,39.8549209631959)) ;
#14831 = CARTESIAN_POINT('Ctrl Pts',(20.1,41.4341904769168,39.8102865715126)) ;
#14832 = CARTESIAN_POINT('Ctrl Pts',(20.1,41.433495615042,39.7656458625524)) ;
#14833 = CARTESIAN_POINT('Ctrl Pts',(20.1,41.4311276841363,39.7210954770712)) ;
#14834 = CARTESIAN_POINT('Ctrl Pts',(20.1,41.4290930699883,39.6828161318511)) ;
#14835 = CARTESIAN_POINT('Ctrl Pts',(20.1,41.4258231001969,39.6446034913311)) ;
#14836 = CARTESIAN_POINT('Ctrl Pts',(20.1,41.4212821252632,39.606522140799)) ;
#14837 = CARTESIAN_POINT('Ctrl Pts',(20.1,41.4199698659409,39.5955173217966)) ;
#14838 = CARTESIAN_POINT('Ctrl Pts',(20.1,41.4185516770161,39.5845261308585)) ;
#14839 = CARTESIAN_POINT('Ctrl Pts',(20.1,41.4170284226326,39.5735605724709)) ;
#14840 = CARTESIAN_POINT('Ctrl Pts',(20.1,41.4080640020682,39.5090277681156)) ;
#14841 = CARTESIAN_POINT('Ctrl Pts',(20.1,41.3954525129461,39.445276444527)) ;
#14842 = CARTESIAN_POINT('Ctrl Pts',(20.1,41.379089864571,39.3825977231924)) ;
#14843 = CARTESIAN_POINT('Ctrl Pts',(20.1,41.3742617457321,39.3641031428327)) ;
#14844 = CARTESIAN_POINT('Ctrl Pts',(20.1,41.3691067076579,39.3457020687507)) ;
#14845 = CARTESIAN_POINT('Ctrl Pts',(20.1,41.3636212695664,39.3274023311227)) ;
#14846 = CARTESIAN_POINT('Ctrl Pts',(20.1,41.3437063393713,39.26096497619)) ;
#14847 = CARTESIAN_POINT('Ctrl Pts',(20.1,41.3194401862383,39.1958601556226)) ;
#14848 = CARTESIAN_POINT('Ctrl Pts',(20.1,41.2910929607224,39.1323838710923)) ;
#14849 = CARTESIAN_POINT('Ctrl Pts',(20.1,41.2781499478771,39.1034013392539)) ;
#14850 = CARTESIAN_POINT('Ctrl Pts',(20.1,41.2643554850943,39.0747588764659)) ;
#14851 = CARTESIAN_POINT('Ctrl Pts',(20.1,41.2497324379344,39.0464878757334)) ;
#14852 = CARTESIAN_POINT('Ctrl Pts',(20.1,41.2363854250346,39.0206838550432)) ;
#14853 = CARTESIAN_POINT('Ctrl Pts',(20.1,41.2223480942368,38.9951893103491)) ;
#14854 = CARTESIAN_POINT('Ctrl Pts',(20.1,41.2076368596568,38.9700298460359)) ;
#14855 = CARTESIAN_POINT('Ctrl Pts',(20.1,41.2020737310709,38.9605156659469)) ;
#14856 = CARTESIAN_POINT('Ctrl Pts',(20.1,41.1964186186447,38.9510569671551)) ;
#14857 = CARTESIAN_POINT('Ctrl Pts',(20.1,41.1906742072217,38.9416571161833)) ;
#14858 = CARTESIAN_POINT('Ctrl Pts',(20.1,41.1568739608253,38.886348181022)) ;
#14859 = CARTESIAN_POINT('Ctrl Pts',(20.1,41.1199697709051,38.8330473189996)) ;
#14860 = CARTESIAN_POINT('Ctrl Pts',(20.1,41.0802042130272,38.7819809617283)) ;
#14861 = CARTESIAN_POINT('Ctrl Pts',(20.1,41.0406084383323,38.7311326375777)) ;
#14862 = CARTESIAN_POINT('Ctrl Pts',(20.1,40.9981747532311,38.6824991338018)) ;
#14863 = CARTESIAN_POINT('Ctrl Pts',(20.1,40.9531114790019,38.6363446012905)) ;
#14864 = CARTESIAN_POINT('Ctrl Pts',(20.1,40.9089802289544,38.5911446629832)) ;
#14865 = CARTESIAN_POINT('Ctrl Pts',(20.1,40.8623261731692,38.5483217771446)) ;
#14866 = CARTESIAN_POINT('Ctrl Pts',(20.1,40.8133282868011,38.5081708244776)) ;
#14867 = CARTESIAN_POINT('Ctrl Pts',(20.1,40.8047841243671,38.5011693742745)) ;
#14868 = CARTESIAN_POINT('Ctrl Pts',(20.1,40.7961686677144,38.4942492979095)) ;
#14869 = CARTESIAN_POINT('Ctrl Pts',(20.1,40.7874828419659,38.4874123235512)) ;
#14870 = CARTESIAN_POINT('Ctrl Pts',(20.1,40.7782551910926,38.4801488561234)) ;
#14871 = CARTESIAN_POINT('Ctrl Pts',(20.1,40.7689549068099,38.4729845740318)) ;
#14872 = CARTESIAN_POINT('Ctrl Pts',(20.1,40.7595878194887,38.4659243469758)) ;
#14873 = CARTESIAN_POINT('Ctrl Pts',(20.1,40.7100628332441,38.4285960253916)) ;
#14874 = CARTESIAN_POINT('Ctrl Pts',(20.1,40.6586327257531,38.3941416234219)) ;
#14875 = CARTESIAN_POINT('Ctrl Pts',(20.1,40.6054916711262,38.3627919275834)) ;
#14876 = CARTESIAN_POINT('Ctrl Pts',(20.1,40.5533162503354,38.3320118916297)) ;
#14877 = CARTESIAN_POINT('Ctrl Pts',(20.1,40.4994906913971,38.3042243928691)) ;
#14878 = CARTESIAN_POINT('Ctrl Pts',(20.1,40.4441860769283,38.2796959625828)) ;
#14879 = CARTESIAN_POINT('Ctrl Pts',(20.1,40.3906414806518,38.2559481268986)) ;
#14880 = CARTESIAN_POINT('Ctrl Pts',(20.1,40.3357098152915,38.2352550726404)) ;
#14881 = CARTESIAN_POINT('Ctrl Pts',(20.1,40.2795449025621,38.2179077161054)) ;
#14882 = CARTESIAN_POINT('Ctrl Pts',(20.1,40.2668745968585,38.2139943064735)) ;
#14883 = CARTESIAN_POINT('Ctrl Pts',(20.1,40.2541415454427,38.2102513721407)) ;
#14884 = CARTESIAN_POINT('Ctrl Pts',(20.1,40.2413475545766,38.2066826248723)) ;
#14885 = CARTESIAN_POINT('Ctrl Pts',(29.6300740822721,38.2459897433641,40.3279613528596)) ;
#14886 = CARTESIAN_POINT('Ctrl Pts',(29.5931358106354,38.4733801681185,40.7908635031756)) ;
#14887 = CARTESIAN_POINT('Ctrl Pts',(29.5192592673619,39.4210811034059,41.4647659628203)) ;
#14888 = CARTESIAN_POINT('Ctrl Pts',(29.4084444524518,41.0530787209739,40.8197841334159)) ;
#14889 = CARTESIAN_POINT('Ctrl Pts',(29.2976296375416,41.3968998908732,39.1007906955674)) ;
#14890 = CARTESIAN_POINT('Ctrl Pts',(29.1868148226315,40.1448501483431,37.8755725352669)) ;
#14891 = CARTESIAN_POINT('Ctrl Pts',(29.0760000077214,38.4342400021641,38.2582535083027)) ;
#14892 = CARTESIAN_POINT('Ctrl Pts',(28.9651851928112,37.8237840021384,39.9011087585314)) ;
#14893 = CARTESIAN_POINT('Ctrl Pts',(28.8543703779011,38.8686165906699,41.3080694099963)) ;
#14894 = CARTESIAN_POINT('Ctrl Pts',(28.7435555629909,40.617802981239,41.1983492914825)) ;
#14895 = CARTESIAN_POINT('Ctrl Pts',(28.6327407480808,41.4786453053513,39.671756482491)) ;
#14896 = CARTESIAN_POINT('Ctrl Pts',(28.5219259331707,40.6674772372708,38.1182099023464)) ;
#14897 = CARTESIAN_POINT('Ctrl Pts',(28.4111111182605,38.9227802986979,37.9521038579512)) ;
#14898 = CARTESIAN_POINT('Ctrl Pts',(28.3002963033504,37.8330223043396,39.324679226451)) ;
#14899 = CARTESIAN_POINT('Ctrl Pts',(28.1894814884402,38.3903556961656,40.9862787943451)) ;
#14900 = CARTESIAN_POINT('Ctrl Pts',(28.0786666735301,40.0873652411245,41.4241133393722)) ;
#14901 = CARTESIAN_POINT('Ctrl Pts',(27.96785185862,41.3790176807763,40.2395580544964)) ;
#14902 = CARTESIAN_POINT('Ctrl Pts',(27.8570370437098,41.0893382026773,38.5110838439939)) ;
#14903 = CARTESIAN_POINT('Ctrl Pts',(27.7462222287997,39.4820628559708,37.812367849582)) ;
#14904 = CARTESIAN_POINT('Ctrl Pts',(27.6354074138896,38.02052476931,38.7795514216669)) ;
#14905 = CARTESIAN_POINT('Ctrl Pts',(27.5245925989794,38.0353711001173,40.5320688312148)) ;
#14906 = CARTESIAN_POINT('Ctrl Pts',(27.4137777840693,39.5130851891104,41.4743526749128)) ;
#14907 = CARTESIAN_POINT('Ctrl Pts',(27.3029629691591,41.1082923469922,40.7485070740931)) ;
#14908 = CARTESIAN_POINT('Ctrl Pts',(27.192148154249,41.3686471870141,39.0153731842676)) ;
#14909 = CARTESIAN_POINT('Ctrl Pts',(27.0813333393388,40.0571114221001,37.8528708534111)) ;
#14910 = CARTESIAN_POINT('Ctrl Pts',(26.9705185244287,38.367763791755,38.3193923515952)) ;
#14911 = CARTESIAN_POINT('Ctrl Pts',(26.8597037095185,37.8386592473608,39.9901963817902)) ;
#14912 = CARTESIAN_POINT('Ctrl Pts',(26.7488888946085,38.9515173907173,41.3441108842142)) ;
#14913 = CARTESIAN_POINT('Ctrl Pts',(26.6380740796983,40.6931441635229,41.1484736934281)) ;
#14914 = CARTESIAN_POINT('Ctrl Pts',(26.5272592647882,41.4778874257816,39.5814013470451)) ;
#14915 = CARTESIAN_POINT('Ctrl Pts',(26.416444449878,40.5912830608963,38.0696241059467)) ;
#14916 = CARTESIAN_POINT('Ctrl Pts',(26.3056296349679,38.8405339270694,37.9895291820938)) ;
#14917 = CARTESIAN_POINT('Ctrl Pts',(26.1948148200577,37.8195975555487,39.4140384490947)) ;
#14918 = CARTESIAN_POINT('Ctrl Pts',(26.0840000051476,38.4579784578276,41.0462172230273)) ;
#14919 = CARTESIAN_POINT('Ctrl Pts',(25.9731851902374,40.1744671234318,41.4000595428663)) ;
#14920 = CARTESIAN_POINT('Ctrl Pts',(25.8623703753273,41.4062982291994,40.1534120973844)) ;
#14921 = CARTESIAN_POINT('Ctrl Pts',(25.7515555604172,41.0319596004962,38.4412764960012)) ;
#14922 = CARTESIAN_POINT('Ctrl Pts',(25.640740745507,39.392265272267,37.822454844445)) ;
#14923 = CARTESIAN_POINT('Ctrl Pts',(25.5299259305969,37.9800636903518,38.8603490676194)) ;
#14924 = CARTESIAN_POINT('Ctrl Pts',(25.4191111156867,38.0810840912803,40.6100154944158)) ;
#14925 = CARTESIAN_POINT('Ctrl Pts',(25.3082963007766,39.6033531444577,41.4784823367307)) ;
#14926 = CARTESIAN_POINT('Ctrl Pts',(25.1974814858665,41.1609314396763,40.6750599193646)) ;
#14927 = CARTESIAN_POINT('Ctrl Pts',(25.0866666709563,41.3357325096837,38.9312186673045)) ;
#14928 = CARTESIAN_POINT('Ctrl Pts',(24.9758518560461,39.9686099201725,37.8346268783008)) ;
#14929 = CARTESIAN_POINT('Ctrl Pts',(24.8650370411361,38.304251048472,38.3836690193557)) ;
#14930 = CARTESIAN_POINT('Ctrl Pts',(24.7542222262259,37.8579600047224,40.0784734419163)) ;
#14931 = CARTESIAN_POINT('Ctrl Pts',(24.6434074113158,39.0360594062455,41.3760170930483)) ;
#14932 = CARTESIAN_POINT('Ctrl Pts',(24.5325925964056,40.7659567397109,41.0949602622614)) ;
#14933 = CARTESIAN_POINT('Ctrl Pts',(24.4217777814955,41.4726788523376,39.4911892118972)) ;
#14934 = CARTESIAN_POINT('Ctrl Pts',(24.3109629665853,40.5127954478126,38.0248462860509)) ;
#14935 = CARTESIAN_POINT('Ctrl Pts',(24.2001481516752,38.7602257828917,38.0309533361934)) ;
#14936 = CARTESIAN_POINT('Ctrl Pts',(24.0893333367651,37.8105848789005,39.5039502404432)) ;
#14937 = CARTESIAN_POINT('Ctrl Pts',(23.9785185218549,38.5284667782912,41.102757078366)) ;
#14938 = CARTESIAN_POINT('Ctrl Pts',(23.8677037069448,40.2602808334951,41.3717511390089)) ;
#14939 = CARTESIAN_POINT('Ctrl Pts',(23.7568888920346,41.4293088255812,40.0660286263046)) ;
#14940 = CARTESIAN_POINT('Ctrl Pts',(23.6460740771245,40.9712172436731,38.3743756391225)) ;
#14941 = CARTESIAN_POINT('Ctrl Pts',(23.5352592622143,39.3030724240549,37.8369460276841)) ;
#14942 = CARTESIAN_POINT('Ctrl Pts',(23.4244444473042,37.9436253671659,38.9430388926739)) ;
#14943 = CARTESIAN_POINT('Ctrl Pts',(23.3136296323941,38.1305753143352,40.6856195776569)) ;
#14944 = CARTESIAN_POINT('Ctrl Pts',(23.2028148174839,39.6937149694595,41.4781674595636)) ;
#14945 = CARTESIAN_POINT('Ctrl Pts',(23.0920000025738,41.2098945632884,40.5991127594935)) ;
#14946 = CARTESIAN_POINT('Ctrl Pts',(22.9811851876637,41.2987187921716,38.848784795215)) ;
#14947 = CARTESIAN_POINT('Ctrl Pts',(22.8703703727535,39.8793182464488,37.8207576467842)) ;
#14948 = CARTESIAN_POINT('Ctrl Pts',(22.7595555578434,38.2439764102052,38.4509915754534)) ;
#14949 = CARTESIAN_POINT('Ctrl Pts',(22.6487407429332,37.8815790320852,40.1656944257316)) ;
#14950 = CARTESIAN_POINT('Ctrl Pts',(22.5379259280231,39.122068318894,41.4037267602073)) ;
#14951 = CARTESIAN_POINT('Ctrl Pts',(22.427111113113,40.8360493115319,41.037930533244)) ;
#14952 = CARTESIAN_POINT('Ctrl Pts',(22.3162962982028,41.4630397864066,39.4013424185359)) ;
#14953 = CARTESIAN_POINT('Ctrl Pts',(22.2054814832927,40.432200557639,37.9839828116129)) ;
#14954 = CARTESIAN_POINT('Ctrl Pts',(22.0946666683825,38.682052148795,38.0762770764856)) ;
#14955 = CARTESIAN_POINT('Ctrl Pts',(21.9838518534724,37.806005117906,39.594196455287)) ;
#14956 = CARTESIAN_POINT('Ctrl Pts',(21.8730370385622,38.6016505653522,41.1557618246954)) ;
#14957 = CARTESIAN_POINT('Ctrl Pts',(21.7622222236521,40.3445983661982,41.3392564020827)) ;
#14958 = CARTESIAN_POINT('Ctrl Pts',(21.6514074087419,41.4479940364311,39.977619430384)) ;
#14959 = CARTESIAN_POINT('Ctrl Pts',(21.5405925938318,40.9072578085518,38.3105427025879)) ;
#14960 = CARTESIAN_POINT('Ctrl Pts',(21.4297777789217,39.2147007747696,37.8558072618482)) ;
#14961 = CARTESIAN_POINT('Ctrl Pts',(21.3189629640115,37.9112968612974,39.0274189154373)) ;
#14962 = CARTESIAN_POINT('Ctrl Pts',(21.2081481491014,38.1837272212218,40.7587017705598)) ;
#14963 = CARTESIAN_POINT('Ctrl Pts',(21.0973333341912,39.7839475036059,41.4734014691738)) ;
#14964 = CARTESIAN_POINT('Ctrl Pts',(20.9865185192811,41.2550721079325,40.520864063088)) ;
#14965 = CARTESIAN_POINT('Ctrl Pts',(20.875703704371,41.257677850447,38.7682418152935)) ;
#14966 = CARTESIAN_POINT('Ctrl Pts',(20.7648888894608,39.7894880096876,37.8113551948838)) ;
#14967 = CARTESIAN_POINT('Ctrl Pts',(20.6540740745507,38.1870148554998,38.5210802763619)) ;
#14968 = CARTESIAN_POINT('Ctrl Pts',(20.5432592596406,37.9096008119324,40.25188160747)) ;
#14969 = CARTESIAN_POINT('Ctrl Pts',(20.4324444447304,39.209052927568,41.4267059761609)) ;
#14970 = CARTESIAN_POINT('Ctrl Pts',(20.3216296298203,40.9038184910527,40.9784637190458)) ;
#14971 = CARTESIAN_POINT('Ctrl Pts',(20.2108148149101,41.4478477610965,39.3100962723047)) ;
#14972 = CARTESIAN_POINT('Ctrl Pts',(20.1369382716367,40.7172822611094,38.4053556254406)) ;
#14973 = CARTESIAN_POINT('Ctrl Pts',(20.1,40.2413475545766,38.2066826248723)) ;
#14974 = CARTESIAN_POINT('Ctrl Pts',(29.5533827215147,38.1267645996105,40.3865280630401)) ;
#14975 = CARTESIAN_POINT('Ctrl Pts',(29.516444449878,38.3735732359292,40.8889601623331)) ;
#14976 = CARTESIAN_POINT('Ctrl Pts',(29.4425679066046,39.402203952147,41.6204111337465)) ;
#14977 = CARTESIAN_POINT('Ctrl Pts',(29.3317530916944,41.1735674864837,40.9203504960237)) ;
#14978 = CARTESIAN_POINT('Ctrl Pts',(29.2209382767843,41.5467495770312,39.0545620544289)) ;
#14979 = CARTESIAN_POINT('Ctrl Pts',(29.1101234618742,40.1877799111328,37.7247152780606)) ;
#14980 = CARTESIAN_POINT('Ctrl Pts',(28.999308646964,38.3310906600031,38.1400756398793)) ;
#14981 = CARTESIAN_POINT('Ctrl Pts',(28.8884938320539,37.6685042161736,39.9232240042654)) ;
#14982 = CARTESIAN_POINT('Ctrl Pts',(28.7776790171437,38.8025612312625,41.4503333366708)) ;
#14983 = CARTESIAN_POINT('Ctrl Pts',(28.6668642022336,40.7011209801604,41.3312435691208)) ;
#14984 = CARTESIAN_POINT('Ctrl Pts',(28.5560493873234,41.6354757153215,39.6742859825908)) ;
#14985 = CARTESIAN_POINT('Ctrl Pts',(28.4452345724133,40.7550372143405,37.9880728831733)) ;
#14986 = CARTESIAN_POINT('Ctrl Pts',(28.3344197575032,38.8613502982639,37.8077820624592)) ;
#14987 = CARTESIAN_POINT('Ctrl Pts',(28.223604942593,37.6785314315704,39.2975697494733)) ;
#14988 = CARTESIAN_POINT('Ctrl Pts',(28.1127901276829,38.283458813891,41.101063119533)) ;
#14989 = CARTESIAN_POINT('Ctrl Pts',(28.0019753127728,40.1253860281235,41.5762869426473)) ;
#14990 = CARTESIAN_POINT('Ctrl Pts',(27.8911604978626,41.5273402993839,40.2905754848318)) ;
#14991 = CARTESIAN_POINT('Ctrl Pts',(27.7803456829525,41.2129233795143,38.4144966514031)) ;
#14992 = CARTESIAN_POINT('Ctrl Pts',(27.6695308680423,39.4683932967824,37.6561131709153)) ;
#14993 = CARTESIAN_POINT('Ctrl Pts',(27.5587160531322,37.8820458396011,38.7058902613705)) ;
#14994 = CARTESIAN_POINT('Ctrl Pts',(27.4479012382221,37.8981599862932,40.6080654846344)) ;
#14995 = CARTESIAN_POINT('Ctrl Pts',(27.3370864233119,39.5020648101976,41.6308165118133)) ;
#14996 = CARTESIAN_POINT('Ctrl Pts',(27.2262716084018,41.2334961301744,40.842986667572)) ;
#14997 = CARTESIAN_POINT('Ctrl Pts',(27.1154567934916,41.5160842079009,38.9618502372781)) ;
#14998 = CARTESIAN_POINT('Ctrl Pts',(27.0046419785815,40.0925486567836,37.7000749654925)) ;
#14999 = CARTESIAN_POINT('Ctrl Pts',(26.8938271636713,38.2589376533124,38.2064354901474)) ;
#15000 = CARTESIAN_POINT('Ctrl Pts',(26.7830123487612,37.6846497464535,40.0199193459146)) ;
#15001 = CARTESIAN_POINT('Ctrl Pts',(26.6721975338511,38.8925414203207,41.489452605269)) ;
#15002 = CARTESIAN_POINT('Ctrl Pts',(26.5613827189409,40.7828959910397,41.2771087991335)) ;
#15003 = CARTESIAN_POINT('Ctrl Pts',(26.4505679040308,41.6346531159385,39.5762148884017)) ;
#15004 = CARTESIAN_POINT('Ctrl Pts',(26.3397530891207,40.6723363671666,37.9353380586228)) ;
#15005 = CARTESIAN_POINT('Ctrl Pts',(26.2289382742105,38.7720804231329,37.8484033561016)) ;
#15006 = CARTESIAN_POINT('Ctrl Pts',(26.1181234593004,37.6639602641803,39.3945598839832)) ;
#15007 = CARTESIAN_POINT('Ctrl Pts',(26.0073086443902,38.3568562826186,41.1661200446965)) ;
#15008 = CARTESIAN_POINT('Ctrl Pts',(25.8964938294801,40.2199260546718,41.5501790503721)) ;
#15009 = CARTESIAN_POINT('Ctrl Pts',(25.78567901457,41.5569504949829,40.197073015578)) ;
#15010 = CARTESIAN_POINT('Ctrl Pts',(25.6748641996598,41.1506448795578,38.3387280416135)) ;
#15011 = CARTESIAN_POINT('Ctrl Pts',(25.5640493847497,39.3709273669721,37.6670615538535)) ;
#15012 = CARTESIAN_POINT('Ctrl Pts',(25.4532345698395,37.8381295501071,38.7935876955824)) ;
#15013 = CARTESIAN_POINT('Ctrl Pts',(25.3424197549294,37.9477766797981,40.6926684738367)) ;
#15014 = CARTESIAN_POINT('Ctrl Pts',(25.2316049400192,39.6000412794646,41.6352988298477)) ;
#15015 = CARTESIAN_POINT('Ctrl Pts',(25.1207901251091,41.2906303859217,40.7632674264492)) ;
#15016 = CARTESIAN_POINT('Ctrl Pts',(25.009975310199,41.4803587518464,38.8705092690112)) ;
#15017 = CARTESIAN_POINT('Ctrl Pts',(24.8991604952888,39.9964894888283,37.6802730295803)) ;
#15018 = CARTESIAN_POINT('Ctrl Pts',(24.7883456803787,38.1900011817109,38.27620112225)) ;
#15019 = CARTESIAN_POINT('Ctrl Pts',(24.6775308654686,37.7055987094957,40.1157349056572)) ;
#15020 = CARTESIAN_POINT('Ctrl Pts',(24.5667160505584,38.9843029779442,41.5240834737454)) ;
#15021 = CARTESIAN_POINT('Ctrl Pts',(24.4559012356483,40.861926463212,41.2190255399759)) ;
#15022 = CARTESIAN_POINT('Ctrl Pts',(24.3450864207381,41.6289997516412,39.4782990061507)) ;
#15023 = CARTESIAN_POINT('Ctrl Pts',(24.234271605828,40.5871462331756,37.8867363961837)) ;
#15024 = CARTESIAN_POINT('Ctrl Pts',(24.1234567909179,38.6849142921439,37.8933649634122)) ;
#15025 = CARTESIAN_POINT('Ctrl Pts',(24.0126419760077,37.6541779418353,39.4921497743036)) ;
#15026 = CARTESIAN_POINT('Ctrl Pts',(23.9018271610976,38.4333640171409,41.2274881722633)) ;
#15027 = CARTESIAN_POINT('Ctrl Pts',(23.7910123461874,40.3130679043387,41.5194532246915)) ;
#15028 = CARTESIAN_POINT('Ctrl Pts',(23.6801975312773,41.5819261021132,40.1022273537289)) ;
#15029 = CARTESIAN_POINT('Ctrl Pts',(23.5693827163671,41.0847153740808,38.2661141253828)) ;
#15030 = CARTESIAN_POINT('Ctrl Pts',(23.4585679014571,39.2741178145893,37.6827902248286)) ;
#15031 = CARTESIAN_POINT('Ctrl Pts',(23.3477530865468,37.7985795432634,38.8833388932469)) ;
#15032 = CARTESIAN_POINT('Ctrl Pts',(23.2369382716368,38.0014942507341,40.7747288363389)) ;
#15033 = CARTESIAN_POINT('Ctrl Pts',(23.1261234567265,39.6981196344702,41.6349570634594)) ;
#15034 = CARTESIAN_POINT('Ctrl Pts',(23.0153086418165,41.343774759884,40.6808346899769)) ;
#15035 = CARTESIAN_POINT('Ctrl Pts',(22.9044938269063,41.440184214356,38.7810358816474)) ;
#15036 = CARTESIAN_POINT('Ctrl Pts',(22.7936790119962,39.8995726716397,37.665219422459)) ;
#15037 = CARTESIAN_POINT('Ctrl Pts',(22.682864197086,38.1245793360405,38.349272749087)) ;
#15038 = CARTESIAN_POINT('Ctrl Pts',(22.5720493821759,37.7312347051225,40.2104042044945)) ;
#15039 = CARTESIAN_POINT('Ctrl Pts',(22.4612345672658,39.0776566996982,41.5541594330641)) ;
#15040 = CARTESIAN_POINT('Ctrl Pts',(22.3504197523556,40.9380046537774,41.1571257055231)) ;
#15041 = CARTESIAN_POINT('Ctrl Pts',(22.2396049374455,41.6185375489323,39.3807796643797)) ;
#15042 = CARTESIAN_POINT('Ctrl Pts',(22.1287901225353,40.4996688692564,37.842383348283)) ;
#15043 = CARTESIAN_POINT('Ctrl Pts',(22.0179753076252,38.6000649496604,37.942559165615)) ;
#15044 = CARTESIAN_POINT('Ctrl Pts',(21.907160492715,37.6492070879968,39.5901026465171)) ;
#15045 = CARTESIAN_POINT('Ctrl Pts',(21.7963456778049,38.5127974000755,41.2850193069807)) ;
#15046 = CARTESIAN_POINT('Ctrl Pts',(21.6855308628947,40.4045858092226,41.484183570233)) ;
#15047 = CARTESIAN_POINT('Ctrl Pts',(21.5747160479846,41.6022069534912,40.0062683743358)) ;
#15048 = CARTESIAN_POINT('Ctrl Pts',(21.4639012330745,41.0152940649862,38.1968301173366)) ;
#15049 = CARTESIAN_POINT('Ctrl Pts',(21.3530864181643,39.1781995881605,37.7032621311913)) ;
#15050 = CARTESIAN_POINT('Ctrl Pts',(21.2422716032542,37.7634903153144,38.9749246245865)) ;
#15051 = CARTESIAN_POINT('Ctrl Pts',(21.131456788344,38.0591851129179,40.8540519493901)) ;
#15052 = CARTESIAN_POINT('Ctrl Pts',(21.0206419734339,39.7960576577108,41.6297840769974)) ;
#15053 = CARTESIAN_POINT('Ctrl Pts',(20.9098271585238,41.3928102819289,40.5959038751708)) ;
#15054 = CARTESIAN_POINT('Ctrl Pts',(20.7990123436136,41.3956385441889,38.6936148609031)) ;
#15055 = CARTESIAN_POINT('Ctrl Pts',(20.6881975287035,39.8020713003344,37.6550140396507)) ;
#15056 = CARTESIAN_POINT('Ctrl Pts',(20.5773827137934,38.062753497707,38.4253467381798)) ;
#15057 = CARTESIAN_POINT('Ctrl Pts',(20.4665678988832,37.7616494302755,40.303951418789)) ;
#15058 = CARTESIAN_POINT('Ctrl Pts',(20.3557530839731,39.1720694379247,41.579100980006)) ;
#15059 = CARTESIAN_POINT('Ctrl Pts',(20.2449382690629,41.0115610438497,41.0925806687903)) ;
#15060 = CARTESIAN_POINT('Ctrl Pts',(20.1341234541528,41.6020481868418,39.2817414707311)) ;
#15061 = CARTESIAN_POINT('Ctrl Pts',(20.0602469108794,40.8090953833627,38.2997396757312)) ;
#15062 = CARTESIAN_POINT('Ctrl Pts',(20.0233086392427,40.2925178008944,38.0841008140837)) ;
#15063 = CARTESIAN_POINT('Ctrl Pts',(29.4766913607574,38.0075394558569,40.4450947732207)) ;
#15064 = CARTESIAN_POINT('Ctrl Pts',(29.4397530891207,38.2737663037398,40.9870568214907)) ;
#15065 = CARTESIAN_POINT('Ctrl Pts',(29.3658765458472,39.3833268008881,41.7760563046727)) ;
#15066 = CARTESIAN_POINT('Ctrl Pts',(29.2550617309371,41.2940562519934,41.0209168586316)) ;
#15067 = CARTESIAN_POINT('Ctrl Pts',(29.1442469160269,41.6965992631892,39.0083334132903)) ;
#15068 = CARTESIAN_POINT('Ctrl Pts',(29.0334321011168,40.2307096739224,37.5738580208544)) ;
#15069 = CARTESIAN_POINT('Ctrl Pts',(28.9226172862067,38.2279413178422,38.0218977714557)) ;
#15070 = CARTESIAN_POINT('Ctrl Pts',(28.8118024712965,37.5132244302088,39.9453392499995)) ;
#15071 = CARTESIAN_POINT('Ctrl Pts',(28.7009876563864,38.7365058718551,41.5925972633453)) ;
#15072 = CARTESIAN_POINT('Ctrl Pts',(28.5901728414763,40.7844389790819,41.4641378467591)) ;
#15073 = CARTESIAN_POINT('Ctrl Pts',(28.4793580265661,41.7923061252916,39.6768154826907)) ;
#15074 = CARTESIAN_POINT('Ctrl Pts',(28.368543211656,40.8425971914102,37.8579358640001)) ;
#15075 = CARTESIAN_POINT('Ctrl Pts',(28.2577283967458,38.7999202978298,37.6634602669672)) ;
#15076 = CARTESIAN_POINT('Ctrl Pts',(28.1469135818357,37.5240405588012,39.2704602724957)) ;
#15077 = CARTESIAN_POINT('Ctrl Pts',(28.0360987669255,38.1765619316163,41.215847444721)) ;
#15078 = CARTESIAN_POINT('Ctrl Pts',(27.9252839520154,40.1634068151226,41.7284605459223)) ;
#15079 = CARTESIAN_POINT('Ctrl Pts',(27.8144691371052,41.6756629179915,40.3415929151672)) ;
#15080 = CARTESIAN_POINT('Ctrl Pts',(27.7036543221951,41.3365085563514,38.3179094588122)) ;
#15081 = CARTESIAN_POINT('Ctrl Pts',(27.592839507285,39.4547237375941,37.4998584922485)) ;
#15082 = CARTESIAN_POINT('Ctrl Pts',(27.4820246923748,37.7435669098921,38.6322291010743)) ;
#15083 = CARTESIAN_POINT('Ctrl Pts',(27.3712098774647,37.7609488724691,40.6840621380539)) ;
#15084 = CARTESIAN_POINT('Ctrl Pts',(27.2603950625546,39.4910444312848,41.7872803487137)) ;
#15085 = CARTESIAN_POINT('Ctrl Pts',(27.1495802476444,41.3586999133566,40.9374662610509)) ;
#15086 = CARTESIAN_POINT('Ctrl Pts',(27.0387654327343,41.6635212287878,38.9083272902888)) ;
#15087 = CARTESIAN_POINT('Ctrl Pts',(26.9279506178241,40.127985891467,37.5472790775738)) ;
#15088 = CARTESIAN_POINT('Ctrl Pts',(26.817135802914,38.1501115148698,38.0934786286996)) ;
#15089 = CARTESIAN_POINT('Ctrl Pts',(26.7063209880039,37.5306402455464,40.049642310039)) ;
#15090 = CARTESIAN_POINT('Ctrl Pts',(26.5955061730937,38.833565449924,41.6347943263239)) ;
#15091 = CARTESIAN_POINT('Ctrl Pts',(26.4846913581836,40.8726478185564,41.4057439048389)) ;
#15092 = CARTESIAN_POINT('Ctrl Pts',(26.3738765432735,41.7914188060955,39.5710284297584)) ;
#15093 = CARTESIAN_POINT('Ctrl Pts',(26.2630617283633,40.7533896734369,37.8010520112989)) ;
#15094 = CARTESIAN_POINT('Ctrl Pts',(26.1522469134532,38.7036269191965,37.7072775301095)) ;
#15095 = CARTESIAN_POINT('Ctrl Pts',(26.041432098543,37.5083229728118,39.3750813188718)) ;
#15096 = CARTESIAN_POINT('Ctrl Pts',(25.9306172836329,38.2557341074098,41.2860228663657)) ;
#15097 = CARTESIAN_POINT('Ctrl Pts',(25.8198024687227,40.2653849859115,41.7002985578778)) ;
#15098 = CARTESIAN_POINT('Ctrl Pts',(25.7089876538126,41.7076027607666,40.2407339337718)) ;
#15099 = CARTESIAN_POINT('Ctrl Pts',(25.5981728389025,41.2693301586193,38.2361795872257)) ;
#15100 = CARTESIAN_POINT('Ctrl Pts',(25.4873580239923,39.3495894616773,37.5116682632619)) ;
#15101 = CARTESIAN_POINT('Ctrl Pts',(25.3765432090822,37.6961954098625,38.7268263235454)) ;
#15102 = CARTESIAN_POINT('Ctrl Pts',(25.265728394172,37.8144692683159,40.7753214532577)) ;
#15103 = CARTESIAN_POINT('Ctrl Pts',(25.1549135792619,39.5967294144714,41.7921153229646)) ;
#15104 = CARTESIAN_POINT('Ctrl Pts',(25.0440987643517,41.4203293321672,40.8514749335338)) ;
#15105 = CARTESIAN_POINT('Ctrl Pts',(24.9332839494416,41.6249849940091,38.8097998707178)) ;
#15106 = CARTESIAN_POINT('Ctrl Pts',(24.8224691345314,40.0243690574841,37.52591918086)) ;
#15107 = CARTESIAN_POINT('Ctrl Pts',(24.7116543196214,38.0757513149498,38.1687332251443)) ;
#15108 = CARTESIAN_POINT('Ctrl Pts',(24.6008395047112,37.5532374142691,40.1529963693981)) ;
#15109 = CARTESIAN_POINT('Ctrl Pts',(24.4900246898011,38.932546549643,41.6721498544424)) ;
#15110 = CARTESIAN_POINT('Ctrl Pts',(24.3792098748909,40.9578961867131,41.3430908176903)) ;
#15111 = CARTESIAN_POINT('Ctrl Pts',(24.2683950599807,41.7853206509447,39.4654088004043)) ;
#15112 = CARTESIAN_POINT('Ctrl Pts',(24.1575802450707,40.6614970185386,37.7486265063164)) ;
#15113 = CARTESIAN_POINT('Ctrl Pts',(24.0467654301604,38.6096028013962,37.755776590631)) ;
#15114 = CARTESIAN_POINT('Ctrl Pts',(23.9359506152504,37.49777100477,39.480349308164)) ;
#15115 = CARTESIAN_POINT('Ctrl Pts',(23.8251358003402,38.3382612559907,41.3522192661607)) ;
#15116 = CARTESIAN_POINT('Ctrl Pts',(23.7143209854301,40.3658549751821,41.6671553103742)) ;
#15117 = CARTESIAN_POINT('Ctrl Pts',(23.6035061705199,41.7345433786454,40.1384260811533)) ;
#15118 = CARTESIAN_POINT('Ctrl Pts',(23.4926913556098,41.1982135044883,38.157852611643)) ;
#15119 = CARTESIAN_POINT('Ctrl Pts',(23.3818765406997,39.2451632051238,37.5286344219733)) ;
#15120 = CARTESIAN_POINT('Ctrl Pts',(23.2710617257895,37.6535337193609,38.8236388938198)) ;
#15121 = CARTESIAN_POINT('Ctrl Pts',(23.1602469108794,37.8724131871331,40.8638380950209)) ;
#15122 = CARTESIAN_POINT('Ctrl Pts',(23.0494320959692,39.702524299481,41.791746667355)) ;
#15123 = CARTESIAN_POINT('Ctrl Pts',(22.9386172810591,41.4776549564797,40.7625566204605)) ;
#15124 = CARTESIAN_POINT('Ctrl Pts',(22.8278024661489,41.5816496365404,38.7132869680797)) ;
#15125 = CARTESIAN_POINT('Ctrl Pts',(22.7169876512388,39.9198270968306,37.5096811981338)) ;
#15126 = CARTESIAN_POINT('Ctrl Pts',(22.6061728363287,38.0051822618756,38.2475539227206)) ;
#15127 = CARTESIAN_POINT('Ctrl Pts',(22.4953580214185,37.58089037816,40.2551139832574)) ;
#15128 = CARTESIAN_POINT('Ctrl Pts',(22.3845432065084,39.0332450805022,41.7045921059208)) ;
#15129 = CARTESIAN_POINT('Ctrl Pts',(22.2737283915983,41.039959996023,41.2763208778023)) ;
#15130 = CARTESIAN_POINT('Ctrl Pts',(22.1629135766881,41.7740353114579,39.3602169102235)) ;
#15131 = CARTESIAN_POINT('Ctrl Pts',(22.052098761778,40.5671371808738,37.7007838849531)) ;
#15132 = CARTESIAN_POINT('Ctrl Pts',(21.9412839468678,38.5180777505257,37.8088412547445)) ;
#15133 = CARTESIAN_POINT('Ctrl Pts',(21.8304691319577,37.4924090580876,39.5860088377472)) ;
#15134 = CARTESIAN_POINT('Ctrl Pts',(21.7196543170475,38.4239442347988,41.414276789266)) ;
#15135 = CARTESIAN_POINT('Ctrl Pts',(21.6088395021374,40.4645732522469,41.6291107383832)) ;
#15136 = CARTESIAN_POINT('Ctrl Pts',(21.4980246872273,41.7564198705513,40.0349173182877)) ;
#15137 = CARTESIAN_POINT('Ctrl Pts',(21.3872098723171,41.1233303214206,38.0831175320853)) ;
#15138 = CARTESIAN_POINT('Ctrl Pts',(21.276395057407,39.1416984015515,37.5507170005344)) ;
#15139 = CARTESIAN_POINT('Ctrl Pts',(21.1655802424968,37.6156837693313,38.9224303337358)) ;
#15140 = CARTESIAN_POINT('Ctrl Pts',(21.0547654275867,37.934643004614,40.9494021282203)) ;
#15141 = CARTESIAN_POINT('Ctrl Pts',(20.9439506126766,39.8081678118156,41.786166684821)) ;
#15142 = CARTESIAN_POINT('Ctrl Pts',(20.8331357977664,41.5305484559254,40.6709436872534)) ;
#15143 = CARTESIAN_POINT('Ctrl Pts',(20.7223209828563,41.5335992379307,38.6189879065129)) ;
#15144 = CARTESIAN_POINT('Ctrl Pts',(20.6115061679461,39.8146545909814,37.4986728844175)) ;
#15145 = CARTESIAN_POINT('Ctrl Pts',(20.500691353036,37.9384921399142,38.3296131999977)) ;
#15146 = CARTESIAN_POINT('Ctrl Pts',(20.3898765381259,37.6136980486187,40.356021230108)) ;
#15147 = CARTESIAN_POINT('Ctrl Pts',(20.2790617232157,39.1350859482812,41.7314959838511)) ;
#15148 = CARTESIAN_POINT('Ctrl Pts',(20.1682469083056,41.1193035966469,41.2066976185349)) ;
#15149 = CARTESIAN_POINT('Ctrl Pts',(20.0574320933954,41.756248612587,39.2533866691575)) ;
#15150 = CARTESIAN_POINT('Ctrl Pts',(19.983555550122,40.9009085056161,38.1941237260219)) ;
#15151 = CARTESIAN_POINT('Ctrl Pts',(19.9466172784853,40.3436880472122,37.9615190032951)) ;
#15152 = CARTESIAN_POINT('Ctrl Pts',(29.4,37.8883143121033,40.5036614834013)) ;
#15153 = CARTESIAN_POINT('Ctrl Pts',(29.3630617283633,38.1739593715505,41.0851534806482)) ;
#15154 = CARTESIAN_POINT('Ctrl Pts',(29.2891851850899,39.3644496496292,41.9317014755988)) ;
#15155 = CARTESIAN_POINT('Ctrl Pts',(29.1783703701797,41.4145450175032,41.1214832212394)) ;
#15156 = CARTESIAN_POINT('Ctrl Pts',(29.0675555552696,41.8464489493472,38.9621047721517)) ;
#15157 = CARTESIAN_POINT('Ctrl Pts',(28.9567407403594,40.2736394367121,37.4230007636482)) ;
#15158 = CARTESIAN_POINT('Ctrl Pts',(28.8459259254493,38.1247919756811,37.9037199030322)) ;
#15159 = CARTESIAN_POINT('Ctrl Pts',(28.7351111105392,37.3579446442441,39.9674544957336)) ;
#15160 = CARTESIAN_POINT('Ctrl Pts',(28.624296295629,38.6704505124476,41.7348611900198)) ;
#15161 = CARTESIAN_POINT('Ctrl Pts',(28.5134814807189,40.8677569780034,41.5970321243973)) ;
#15162 = CARTESIAN_POINT('Ctrl Pts',(28.4026666658087,41.9491365352617,39.6793449827905)) ;
#15163 = CARTESIAN_POINT('Ctrl Pts',(28.2918518508986,40.9301571684799,37.7277988448269)) ;
#15164 = CARTESIAN_POINT('Ctrl Pts',(28.1810370359885,38.7384902973957,37.5191384714753)) ;
#15165 = CARTESIAN_POINT('Ctrl Pts',(28.0702222210783,37.369549686032,39.2433507955181)) ;
#15166 = CARTESIAN_POINT('Ctrl Pts',(27.9594074061682,38.0696650493416,41.330631769909)) ;
#15167 = CARTESIAN_POINT('Ctrl Pts',(27.8485925912581,40.2014276021217,41.8806341491974)) ;
#15168 = CARTESIAN_POINT('Ctrl Pts',(27.7377777763479,41.8239855365992,40.3926103455026)) ;
#15169 = CARTESIAN_POINT('Ctrl Pts',(27.6269629614378,41.4600937331885,38.2213222662214)) ;
#15170 = CARTESIAN_POINT('Ctrl Pts',(27.5161481465276,39.4410541784057,37.3436038135818)) ;
#15171 = CARTESIAN_POINT('Ctrl Pts',(27.4053333316175,37.6050879801832,38.5585679407779)) ;
#15172 = CARTESIAN_POINT('Ctrl Pts',(27.2945185167073,37.623737758645,40.7600587914735)) ;
#15173 = CARTESIAN_POINT('Ctrl Pts',(27.1837037017972,39.4800240523721,41.9437441856142)) ;
#15174 = CARTESIAN_POINT('Ctrl Pts',(27.072888886887,41.4839036965388,41.0319458545299)) ;
#15175 = CARTESIAN_POINT('Ctrl Pts',(26.9620740719769,41.8109582496746,38.8548043432993)) ;
#15176 = CARTESIAN_POINT('Ctrl Pts',(26.8512592570668,40.1634231261504,37.3944831896552)) ;
#15177 = CARTESIAN_POINT('Ctrl Pts',(26.7404444421566,38.0412853764272,37.9805217672518)) ;
#15178 = CARTESIAN_POINT('Ctrl Pts',(26.6296296272465,37.3766307446391,40.0793652741634)) ;
#15179 = CARTESIAN_POINT('Ctrl Pts',(26.5188148123364,38.7745894795274,41.7801360473788)) ;
#15180 = CARTESIAN_POINT('Ctrl Pts',(26.4079999974262,40.9623996460732,41.5343790105443)) ;
#15181 = CARTESIAN_POINT('Ctrl Pts',(26.2971851825161,41.9481844962523,39.565841971115)) ;
#15182 = CARTESIAN_POINT('Ctrl Pts',(26.1863703676059,40.8344429797072,37.666765963975)) ;
#15183 = CARTESIAN_POINT('Ctrl Pts',(26.0755555526958,38.63517341526,37.5661517041173)) ;
#15184 = CARTESIAN_POINT('Ctrl Pts',(25.9647407377857,37.3526856814434,39.3556027537603)) ;
#15185 = CARTESIAN_POINT('Ctrl Pts',(25.8539259228755,38.1546119322008,41.405925688035)) ;
#15186 = CARTESIAN_POINT('Ctrl Pts',(25.7431111079654,40.3108439171514,41.8504180653835)) ;
#15187 = CARTESIAN_POINT('Ctrl Pts',(25.6322962930553,41.8582550265502,40.2843948519655)) ;
#15188 = CARTESIAN_POINT('Ctrl Pts',(25.5214814781451,41.3880154376809,38.133631132838)) ;
#15189 = CARTESIAN_POINT('Ctrl Pts',(25.410666663235,39.3282515563825,37.3562749726704)) ;
#15190 = CARTESIAN_POINT('Ctrl Pts',(25.2998518483248,37.5542612696178,38.6600649515084)) ;
#15191 = CARTESIAN_POINT('Ctrl Pts',(25.1890370334147,37.6811618568337,40.8579744326787)) ;
#15192 = CARTESIAN_POINT('Ctrl Pts',(25.0782222185045,39.5934175494783,41.9489318160816)) ;
#15193 = CARTESIAN_POINT('Ctrl Pts',(24.9674074035944,41.5500282784125,40.9396824406184)) ;
#15194 = CARTESIAN_POINT('Ctrl Pts',(24.8565925886842,41.7696112361718,38.7490904724245)) ;
#15195 = CARTESIAN_POINT('Ctrl Pts',(24.7457777737741,40.0522486261398,37.3715653321395)) ;
#15196 = CARTESIAN_POINT('Ctrl Pts',(24.634962958864,37.9615014481887,38.0612653280387)) ;
#15197 = CARTESIAN_POINT('Ctrl Pts',(24.5241481439539,37.4008761190426,40.190257833139)) ;
#15198 = CARTESIAN_POINT('Ctrl Pts',(24.4133333290437,38.8807901213416,41.8202162351395)) ;
#15199 = CARTESIAN_POINT('Ctrl Pts',(24.3025185141336,41.0538659102142,41.4671560954048)) ;
#15200 = CARTESIAN_POINT('Ctrl Pts',(24.1917036992234,41.9416415502482,39.4525185946579)) ;
#15201 = CARTESIAN_POINT('Ctrl Pts',(24.0808888843133,40.7358478039017,37.6105166164492)) ;
#15202 = CARTESIAN_POINT('Ctrl Pts',(23.9700740694031,38.5342913106484,37.6181882178497)) ;
#15203 = CARTESIAN_POINT('Ctrl Pts',(23.859259254493,37.3413640677048,39.4685488420246)) ;
#15204 = CARTESIAN_POINT('Ctrl Pts',(23.7484444395828,38.2431584948403,41.4769503600581)) ;
#15205 = CARTESIAN_POINT('Ctrl Pts',(23.6376296246727,40.4186420460256,41.8148573960569)) ;
#15206 = CARTESIAN_POINT('Ctrl Pts',(23.5268148097626,41.8871606551775,40.1746248085776)) ;
#15207 = CARTESIAN_POINT('Ctrl Pts',(23.4159999948524,41.311711634896,38.0495910979033)) ;
#15208 = CARTESIAN_POINT('Ctrl Pts',(23.3051851799423,39.2162085956582,37.3744786191179)) ;
#15209 = CARTESIAN_POINT('Ctrl Pts',(23.1943703650321,37.5084878954584,38.7639388943928)) ;
#15210 = CARTESIAN_POINT('Ctrl Pts',(23.083555550122,37.743332123532,40.9529473537028)) ;
#15211 = CARTESIAN_POINT('Ctrl Pts',(22.9727407352119,39.7069289644918,41.9485362712508)) ;
#15212 = CARTESIAN_POINT('Ctrl Pts',(22.8619259203017,41.6115351530753,40.844278550944)) ;
#15213 = CARTESIAN_POINT('Ctrl Pts',(22.7511111053916,41.7231150587249,38.645538054512)) ;
#15214 = CARTESIAN_POINT('Ctrl Pts',(22.6402962904815,39.9400815220214,37.3541429738087)) ;
#15215 = CARTESIAN_POINT('Ctrl Pts',(22.5294814755713,37.8857851877109,38.1458350963543)) ;
#15216 = CARTESIAN_POINT('Ctrl Pts',(22.4186666606612,37.4305460511974,40.2998237620203)) ;
#15217 = CARTESIAN_POINT('Ctrl Pts',(22.307851845751,38.9888334613064,41.8550247787775)) ;
#15218 = CARTESIAN_POINT('Ctrl Pts',(22.1970370308409,41.1419153382684,41.3955160500816)) ;
#15219 = CARTESIAN_POINT('Ctrl Pts',(22.0862222159308,41.9295330739837,39.3396541560672)) ;
#15220 = CARTESIAN_POINT('Ctrl Pts',(21.9754074010206,40.6346054924911,37.5591844216232)) ;
#15221 = CARTESIAN_POINT('Ctrl Pts',(21.8645925861105,38.4360905513911,37.675123343874)) ;
#15222 = CARTESIAN_POINT('Ctrl Pts',(21.7537777712003,37.3356110281783,39.5819150289772)) ;
#15223 = CARTESIAN_POINT('Ctrl Pts',(21.6429629562902,38.3350910695221,41.5435342715513)) ;
#15224 = CARTESIAN_POINT('Ctrl Pts',(21.53214814138,40.5245606952712,41.7740379065334)) ;
#15225 = CARTESIAN_POINT('Ctrl Pts',(21.4213333264699,41.9106327876115,40.0635662622395)) ;
#15226 = CARTESIAN_POINT('Ctrl Pts',(21.3105185115598,41.2313665778549,37.9694049468339)) ;
#15227 = CARTESIAN_POINT('Ctrl Pts',(21.1997036966496,39.1051972149425,37.3981718698776)) ;
#15228 = CARTESIAN_POINT('Ctrl Pts',(21.0888888817395,37.4678772233483,38.869936042885)) ;
#15229 = CARTESIAN_POINT('Ctrl Pts',(20.9780740668294,37.8101008963102,41.0447523070506)) ;
#15230 = CARTESIAN_POINT('Ctrl Pts',(20.8672592519192,39.8202779659203,41.9425492926447)) ;
#15231 = CARTESIAN_POINT('Ctrl Pts',(20.7564444370091,41.6682866299218,40.7459834993361)) ;
#15232 = CARTESIAN_POINT('Ctrl Pts',(20.6456296220989,41.6715599316725,38.5443609521226)) ;
#15233 = CARTESIAN_POINT('Ctrl Pts',(20.5348148071888,39.8272378816283,37.3423317291844)) ;
#15234 = CARTESIAN_POINT('Ctrl Pts',(20.4239999922786,37.8142307821214,38.2338796618157)) ;
#15235 = CARTESIAN_POINT('Ctrl Pts',(20.3131851773685,37.4657466669618,40.4080910414269)) ;
#15236 = CARTESIAN_POINT('Ctrl Pts',(20.2023703624584,39.0981024586378,41.8838909876963)) ;
#15237 = CARTESIAN_POINT('Ctrl Pts',(20.0915555475482,41.227046149444,41.3208145682793)) ;
#15238 = CARTESIAN_POINT('Ctrl Pts',(19.9807407326381,41.9104490383323,39.2250318675839)) ;
#15239 = CARTESIAN_POINT('Ctrl Pts',(19.9068641893647,40.9927216278695,38.0885077763125)) ;
#15240 = CARTESIAN_POINT('Ctrl Pts',(19.8699259177279,40.39485829353,37.8389371925064)) ;
#15241 = CARTESIAN_POINT('Ctrl Pts',(20.1758696921242,39.6403856614379,41.5960667040991)) ;
#15242 = CARTESIAN_POINT('Ctrl Pts',(20.1505797947495,40.0840112824575,41.5922443072459)) ;
#15243 = CARTESIAN_POINT('Ctrl Pts',(20.1252898973747,40.5301478361562,41.4385916227714)) ;
#15244 = CARTESIAN_POINT('Ctrl Pts',(20.1,40.8749138146614,41.1621829179884)) ;
#15245 = CARTESIAN_POINT('',(29.4,40.9082616204537,40.5457424023813)) ;
#15246 = CARTESIAN_POINT('Ctrl Pts',(29.4,40.9099017087087,40.5477081290461)) ;
#15247 = CARTESIAN_POINT('Ctrl Pts',(29.4,40.8911935153115,40.5827280609995)) ;
#15248 = CARTESIAN_POINT('Ctrl Pts',(29.4,40.8710967810982,40.6169137862787)) ;
#15249 = CARTESIAN_POINT('Ctrl Pts',(29.4,40.849630844981,40.650172378807)) ;
#15250 = CARTESIAN_POINT('Ctrl Pts',(29.4,40.8174332982874,40.7000581643625)) ;
#15251 = CARTESIAN_POINT('Ctrl Pts',(29.4,40.7821579182634,40.7478593980477)) ;
#15252 = CARTESIAN_POINT('Ctrl Pts',(29.4,40.7441238056603,40.7934984035053)) ;
#15253 = CARTESIAN_POINT('Ctrl Pts',(29.4,40.720671405954,40.8216400932919)) ;
#15254 = CARTESIAN_POINT('Ctrl Pts',(29.4,40.6961690606009,40.8489593935245)) ;
#15255 = CARTESIAN_POINT('Ctrl Pts',(29.4,40.6706828011567,40.875434378279)) ;
#15256 = CARTESIAN_POINT('Ctrl Pts',(29.4,40.6617631345853,40.8847000783717)) ;
#15257 = CARTESIAN_POINT('Ctrl Pts',(29.4,40.6527245408652,40.89386049634)) ;
#15258 = CARTESIAN_POINT('Ctrl Pts',(29.4,40.6435778736667,40.902907120743)) ;
#15259 = CARTESIAN_POINT('Ctrl Pts',(29.4,40.5992766463879,40.9467237979089)) ;
#15260 = CARTESIAN_POINT('Ctrl Pts',(29.4,40.5523942995144,40.9879249952783)) ;
#15261 = CARTESIAN_POINT('Ctrl Pts',(29.4,40.5032793806035,41.0264241184463)) ;
#15262 = CARTESIAN_POINT('Ctrl Pts',(29.4,40.465416175545,41.0561034954543)) ;
#15263 = CARTESIAN_POINT('Ctrl Pts',(29.4,40.4262249186537,41.0841767525349)) ;
#15264 = CARTESIAN_POINT('Ctrl Pts',(29.4,40.3858469011584,41.1105939537831)) ;
#15265 = CARTESIAN_POINT('Ctrl Pts',(29.4,40.3698454319037,41.1210628687965)) ;
#15266 = CARTESIAN_POINT('Ctrl Pts',(29.4,40.3536574290092,41.131271591281)) ;
#15267 = CARTESIAN_POINT('Ctrl Pts',(29.4,40.3372911151227,41.1412165309672)) ;
#15268 = CARTESIAN_POINT('Ctrl Pts',(29.4,40.3267725201988,41.1476081224291)) ;
#15269 = CARTESIAN_POINT('Ctrl Pts',(29.4,40.3161801620067,41.1538906909963)) ;
#15270 = CARTESIAN_POINT('Ctrl Pts',(29.4,40.3055290468822,41.1600561153331)) ;
#15271 = CARTESIAN_POINT('Ctrl Pts',(29.4,40.2495545026299,41.1924571187342)) ;
#15272 = CARTESIAN_POINT('Ctrl Pts',(29.4,40.1918758690529,41.2216774859145)) ;
#15273 = CARTESIAN_POINT('Ctrl Pts',(29.4,40.1328473057965,41.2476277355336)) ;
#15274 = CARTESIAN_POINT('Ctrl Pts',(29.4,40.0725752515564,41.2741246510318)) ;
#15275 = CARTESIAN_POINT('Ctrl Pts',(29.4,40.0108950153682,41.2972129741303)) ;
#15276 = CARTESIAN_POINT('Ctrl Pts',(29.4,39.9481419144707,41.3167635433489)) ;
#15277 = CARTESIAN_POINT('Ctrl Pts',(29.4,39.9063144539236,41.3297947824584)) ;
#15278 = CARTESIAN_POINT('Ctrl Pts',(29.4,39.8640094931252,41.3412535685766)) ;
#15279 = CARTESIAN_POINT('Ctrl Pts',(29.4,39.8213191168389,41.3510910041002)) ;
#15280 = CARTESIAN_POINT('Ctrl Pts',(29.4,39.8000975814559,41.3559812277103)) ;
#15281 = CARTESIAN_POINT('Ctrl Pts',(29.4,39.7787807324178,41.3604706528433)) ;
#15282 = CARTESIAN_POINT('Ctrl Pts',(29.4,39.7573795302911,41.3645523656715)) ;
#15283 = CARTESIAN_POINT('Ctrl Pts',(29.4,39.742623604249,41.3673666679832)) ;
#15284 = CARTESIAN_POINT('Ctrl Pts',(29.4,39.7278275724937,41.3699871322496)) ;
#15285 = CARTESIAN_POINT('Ctrl Pts',(29.4,39.7129949834893,41.3724113112808)) ;
#15286 = CARTESIAN_POINT('Ctrl Pts',(29.4,39.7024878196002,41.3741285601285)) ;
#15287 = CARTESIAN_POINT('Ctrl Pts',(29.4,39.6919717860519,41.3757457576257)) ;
#15288 = CARTESIAN_POINT('Ctrl Pts',(29.4,39.6814484822052,41.3772624926511)) ;
#15289 = CARTESIAN_POINT('Ctrl Pts',(29.4,39.6144049308324,41.3869255513325)) ;
#15290 = CARTESIAN_POINT('Ctrl Pts',(29.4,39.5470667639266,41.3925146504903)) ;
#15291 = CARTESIAN_POINT('Ctrl Pts',(29.4,39.4797876237661,41.39390686565)) ;
#15292 = CARTESIAN_POINT('Ctrl Pts',(29.4,39.4636730092403,41.3942403272635)) ;
#15293 = CARTESIAN_POINT('Ctrl Pts',(29.4,39.4475616490742,41.3943328224262)) ;
#15294 = CARTESIAN_POINT('Ctrl Pts',(29.4,39.4314581800028,41.3941822776708)) ;
#15295 = CARTESIAN_POINT('Ctrl Pts',(29.4,39.3665783523775,41.3935757426604)) ;
#15296 = CARTESIAN_POINT('Ctrl Pts',(29.4,39.3018273724191,41.3890282454472)) ;
#15297 = CARTESIAN_POINT('Ctrl Pts',(29.4,39.2374411018851,41.3807559085843)) ;
#15298 = CARTESIAN_POINT('Ctrl Pts',(29.4,39.2024146503065,41.3762557161649)) ;
#15299 = CARTESIAN_POINT('Ctrl Pts',(29.4,39.1674959422765,41.3706522775741)) ;
#15300 = CARTESIAN_POINT('Ctrl Pts',(29.4,39.1327223454014,41.3639741186901)) ;
#15301 = CARTESIAN_POINT('Ctrl Pts',(29.4,39.1026495332469,41.358198730588)) ;
#15302 = CARTESIAN_POINT('Ctrl Pts',(29.4,39.0726852321098,41.351619475739)) ;
#15303 = CARTESIAN_POINT('Ctrl Pts',(29.4,39.0428537605999,41.3442522807742)) ;
#15304 = CARTESIAN_POINT('Ctrl Pts',(29.4,39.0327852838907,41.3417657647841)) ;
#15305 = CARTESIAN_POINT('Ctrl Pts',(29.4,39.0227348244623,41.339190133892)) ;
#15306 = CARTESIAN_POINT('Ctrl Pts',(29.4,39.0127114014828,41.3365283979405)) ;
#15307 = CARTESIAN_POINT('Ctrl Pts',(29.4,38.9471470175288,41.3191176712587)) ;
#15308 = CARTESIAN_POINT('Ctrl Pts',(29.4,38.8826389394181,41.2980024905982)) ;
#15309 = CARTESIAN_POINT('Ctrl Pts',(29.4,38.8194432421882,41.2734401520375)) ;
#15310 = CARTESIAN_POINT('Ctrl Pts',(29.4,38.7549205183317,41.2483620366326)) ;
#15311 = CARTESIAN_POINT('Ctrl Pts',(29.4,38.6917649898121,41.2196903008299)) ;
#15312 = CARTESIAN_POINT('Ctrl Pts',(29.4,38.6302461565059,41.1876436249062)) ;
#15313 = CARTESIAN_POINT('Ctrl Pts',(29.4,38.5682684460675,41.155357908579)) ;
#15314 = CARTESIAN_POINT('Ctrl Pts',(29.4,38.5079509547186,41.1196463915286)) ;
#15315 = CARTESIAN_POINT('Ctrl Pts',(29.4,38.4495803765141,41.0806812192905)) ;
#15316 = CARTESIAN_POINT('Ctrl Pts',(29.4,38.4345977593732,41.0706796007452)) ;
#15317 = CARTESIAN_POINT('Ctrl Pts',(29.4,38.4197435148233,41.0604633668381)) ;
#15318 = CARTESIAN_POINT('Ctrl Pts',(29.4,38.4050227327501,41.0500349287453)) ;
#15319 = CARTESIAN_POINT('Ctrl Pts',(29.4,38.395076102545,41.0429885763974)) ;
#15320 = CARTESIAN_POINT('Ctrl Pts',(29.4,38.3851898915416,41.035844847252)) ;
#15321 = CARTESIAN_POINT('Ctrl Pts',(29.4,38.3753786911808,41.0286143383668)) ;
#15322 = CARTESIAN_POINT('Ctrl Pts',(29.4,38.3172621602953,40.985784503332)) ;
#15323 = CARTESIAN_POINT('Ctrl Pts',(29.4,38.2616662256681,40.9398368489584)) ;
#15324 = CARTESIAN_POINT('Ctrl Pts',(29.4,38.2088717556074,40.8910128665259)) ;
#15325 = CARTESIAN_POINT('Ctrl Pts',(29.4,38.1559526948364,40.8420736634151)) ;
#15326 = CARTESIAN_POINT('Ctrl Pts',(29.4,38.1058473267557,40.7902441084932)) ;
#15327 = CARTESIAN_POINT('Ctrl Pts',(29.4,38.0588546893559,40.7357177820414)) ;
#15328 = CARTESIAN_POINT('Ctrl Pts',(29.4,38.0128654690254,40.6823557368411)) ;
#15329 = CARTESIAN_POINT('Ctrl Pts',(29.4,37.9698566114721,40.6264102871568)) ;
#15330 = CARTESIAN_POINT('Ctrl Pts',(29.4,37.9301375288794,40.5680230943791)) ;
#15331 = CARTESIAN_POINT('Ctrl Pts',(29.4,37.9157597103701,40.5468876499976)) ;
#15332 = CARTESIAN_POINT('Ctrl Pts',(29.4,37.9018133110483,40.5254319089879)) ;
#15333 = CARTESIAN_POINT('Ctrl Pts',(29.4,37.8883143121033,40.5036614834013)) ;
#15334 = CARTESIAN_POINT('Ctrl Pts',(29.4,40.9099017087087,40.5477081290461)) ;
#15335 = CARTESIAN_POINT('Ctrl Pts',(29.3658765458472,41.1836081239267,40.1599355816674)) ;
#15336 = CARTESIAN_POINT('Ctrl Pts',(29.2948148200577,41.3650964581925,39.0696688144179)) ;
#15337 = CARTESIAN_POINT('Ctrl Pts',(29.1868148226315,40.1448501483431,37.8755725352669)) ;
#15338 = CARTESIAN_POINT('Ctrl Pts',(29.0760000077214,38.4342400021641,38.2582535083027)) ;
#15339 = CARTESIAN_POINT('Ctrl Pts',(28.9651851928112,37.8237840021384,39.9011087585314)) ;
#15340 = CARTESIAN_POINT('Ctrl Pts',(28.8751664483696,38.6725380053612,41.044032034868)) ;
#15341 = CARTESIAN_POINT('Ctrl Pts',(28.8220859755646,39.4154275518878,41.1959818279421)) ;
#15342 = CARTESIAN_POINT('Ctrl Pts',(28.8059437743963,39.6416116368869,41.195305032435)) ;
#15343 = CARTESIAN_POINT('Origin',(29.4,39.642135623731,39.642135623731)) ;
#15344 = CARTESIAN_POINT('',(29.4,39.642135623731,41.596135623731)) ;
#15345 = CARTESIAN_POINT('Origin',(29.4,39.642135623731,39.642135623731)) ;
#15346 = CARTESIAN_POINT('',(29.4,40.9082616204539,38.7385288450808)) ;
#15347 = CARTESIAN_POINT('Ctrl Pts',(29.4,37.8858801137886,38.7785081419809)) ;
#15348 = CARTESIAN_POINT('Ctrl Pts',(29.4,37.9116490910512,38.7365164424919)) ;
#15349 = CARTESIAN_POINT('Ctrl Pts',(29.4,37.9390708494547,38.6956362623256)) ;
#15350 = CARTESIAN_POINT('Ctrl Pts',(29.4,37.9681504858012,38.6559804743706)) ;
#15351 = CARTESIAN_POINT('Ctrl Pts',(29.4,38.0106510442209,38.5980226267355)) ;
#15352 = CARTESIAN_POINT('Ctrl Pts',(29.4,38.0566920308732,38.5426781003507)) ;
#15353 = CARTESIAN_POINT('Ctrl Pts',(29.4,38.1059332588112,38.490108579696)) ;
#15354 = CARTESIAN_POINT('Ctrl Pts',(29.4,38.1306294723998,38.4637431098508)) ;
#15355 = CARTESIAN_POINT('Ctrl Pts',(29.4,38.1561311460157,38.4380763320497)) ;
#15356 = CARTESIAN_POINT('Ctrl Pts',(29.4,38.1823975605347,38.4131329663715)) ;
#15357 = CARTESIAN_POINT('Ctrl Pts',(29.4,38.1930192567399,38.4030462888625)) ;
#15358 = CARTESIAN_POINT('Ctrl Pts',(29.4,38.2037677831062,38.3930763509752)) ;
#15359 = CARTESIAN_POINT('Ctrl Pts',(29.4,38.2146347705142,38.3832300940798)) ;
#15360 = CARTESIAN_POINT('Ctrl Pts',(29.4,38.2675074522367,38.335323716034)) ;
#15361 = CARTESIAN_POINT('Ctrl Pts',(29.4,38.3230763648864,38.2904355096495)) ;
#15362 = CARTESIAN_POINT('Ctrl Pts',(29.4,38.3810032036924,38.2487185952537)) ;
#15363 = CARTESIAN_POINT('Ctrl Pts',(29.4,38.4238104588198,38.2178902843278)) ;
#15364 = CARTESIAN_POINT('Ctrl Pts',(29.4,38.4679061537415,38.1887947021649)) ;
#15365 = CARTESIAN_POINT('Ctrl Pts',(29.4,38.5131601184473,38.1615107790893)) ;
#15366 = CARTESIAN_POINT('Ctrl Pts',(29.4,38.5369340087092,38.1471773389735)) ;
#15367 = CARTESIAN_POINT('Ctrl Pts',(29.4,38.561027626749,38.1333441438862)) ;
#15368 = CARTESIAN_POINT('Ctrl Pts',(29.4,38.5854223149118,38.1200243793908)) ;
#15369 = CARTESIAN_POINT('Ctrl Pts',(29.4,38.5965922808676,38.11392545675)) ;
#15370 = CARTESIAN_POINT('Ctrl Pts',(29.4,38.6078253694791,38.1079341964166)) ;
#15371 = CARTESIAN_POINT('Ctrl Pts',(29.4,38.6191197890281,38.102051951947)) ;
#15372 = CARTESIAN_POINT('Ctrl Pts',(29.4,38.6299426725146,38.0964152880833)) ;
#15373 = CARTESIAN_POINT('Ctrl Pts',(29.4,38.640812808894,38.0908834475283)) ;
#15374 = CARTESIAN_POINT('Ctrl Pts',(29.4,38.6517284773785,38.0854570976242)) ;
#15375 = CARTESIAN_POINT('Ctrl Pts',(29.4,38.7140552839742,38.054473465108)) ;
#15376 = CARTESIAN_POINT('Ctrl Pts',(29.4,38.7778654686989,38.0269249898323)) ;
#15377 = CARTESIAN_POINT('Ctrl Pts',(29.4,38.8428505039851,38.002963908533)) ;
#15378 = CARTESIAN_POINT('Ctrl Pts',(29.4,38.9062492642292,37.979587713663)) ;
#15379 = CARTESIAN_POINT('Ctrl Pts',(29.4,38.9707671925793,37.9596258261471)) ;
#15380 = CARTESIAN_POINT('Ctrl Pts',(29.4,39.0361228154364,37.9432679613406)) ;
#15381 = CARTESIAN_POINT('Ctrl Pts',(29.4,39.079431002153,37.9324283513369)) ;
#15382 = CARTESIAN_POINT('Ctrl Pts',(29.4,39.1231071037785,37.9231722948001)) ;
#15383 = CARTESIAN_POINT('Ctrl Pts',(29.4,39.1670674387888,37.9155674593897)) ;
#15384 = CARTESIAN_POINT('Ctrl Pts',(29.4,39.2048397834777,37.9090331037176)) ;
#15385 = CARTESIAN_POINT('Ctrl Pts',(29.4,39.2428219878473,37.9037179738841)) ;
#15386 = CARTESIAN_POINT('Ctrl Pts',(29.4,39.280959018589,37.8996711971933)) ;
#15387 = CARTESIAN_POINT('Ctrl Pts',(29.4,39.2919799253728,37.8985017524878)) ;
#15388 = CARTESIAN_POINT('Ctrl Pts',(29.4,39.3030111173088,37.8974386139797)) ;
#15389 = CARTESIAN_POINT('Ctrl Pts',(29.4,39.3140406985631,37.8964836104455)) ;
#15390 = CARTESIAN_POINT('Ctrl Pts',(29.4,39.3789502991843,37.89086337006)) ;
#15391 = CARTESIAN_POINT('Ctrl Pts',(29.4,39.4439095597764,37.8889726547203)) ;
#15392 = CARTESIAN_POINT('Ctrl Pts',(29.4,39.5086578198928,37.8909777261666)) ;
#15393 = CARTESIAN_POINT('Ctrl Pts',(29.4,39.5277630833133,37.891569362422)) ;
#15394 = CARTESIAN_POINT('Ctrl Pts',(29.4,39.5468499309991,37.8925005294073)) ;
#15395 = CARTESIAN_POINT('Ctrl Pts',(29.4,39.5659115036032,37.8937763630377)) ;
#15396 = CARTESIAN_POINT('Ctrl Pts',(29.4,39.6351147135408,37.8984082884514)) ;
#15397 = CARTESIAN_POINT('Ctrl Pts',(29.4,39.7039870331875,37.9075788728914)) ;
#15398 = CARTESIAN_POINT('Ctrl Pts',(29.4,39.7721797673507,37.9210906044853)) ;
#15399 = CARTESIAN_POINT('Ctrl Pts',(29.4,39.8033157439461,37.9272598975022)) ;
#15400 = CARTESIAN_POINT('Ctrl Pts',(29.4,39.8343096425566,37.93433496609)) ;
#15401 = CARTESIAN_POINT('Ctrl Pts',(29.4,39.8651257692214,37.9423005035321)) ;
#15402 = CARTESIAN_POINT('Ctrl Pts',(29.4,39.8932532269645,37.9495710576884)) ;
#15403 = CARTESIAN_POINT('Ctrl Pts',(29.4,39.9212325733677,37.9575835088157)) ;
#15404 = CARTESIAN_POINT('Ctrl Pts',(29.4,39.9490351922892,37.9663275513776)) ;
#15405 = CARTESIAN_POINT('Ctrl Pts',(29.4,39.9595483179186,37.9696339743525)) ;
#15406 = CARTESIAN_POINT('Ctrl Pts',(29.4,39.9700278224812,37.9730424119132)) ;
#15407 = CARTESIAN_POINT('Ctrl Pts',(29.4,39.980469829338,37.9765509966401)) ;
#15408 = CARTESIAN_POINT('Ctrl Pts',(29.4,40.0419133031625,37.997196418232)) ;
#15409 = CARTESIAN_POINT('Ctrl Pts',(29.4,40.1020897414224,38.021314799644)) ;
#15410 = CARTESIAN_POINT('Ctrl Pts',(29.4,40.1607244120033,38.0487200327042)) ;
#15411 = CARTESIAN_POINT('Ctrl Pts',(29.4,40.219108739998,38.0760082582524)) ;
#15412 = CARTESIAN_POINT('Ctrl Pts',(29.4,40.2759652711504,38.1065560863141)) ;
#15413 = CARTESIAN_POINT('Ctrl Pts',(29.4,40.3309901219769,38.1402191974643)) ;
#15414 = CARTESIAN_POINT('Ctrl Pts',(29.4,40.3848769210849,38.1731860711705)) ;
#15415 = CARTESIAN_POINT('Ctrl Pts',(29.4,40.437007641609,38.2091414431635)) ;
#15416 = CARTESIAN_POINT('Ctrl Pts',(29.4,40.4870549707429,38.2479764423802)) ;
#15417 = CARTESIAN_POINT('Ctrl Pts',(29.4,40.4957821815725,38.2547484566234)) ;
#15418 = CARTESIAN_POINT('Ctrl Pts',(29.4,40.5044459225108,38.2616080859552)) ;
#15419 = CARTESIAN_POINT('Ctrl Pts',(29.4,40.5130443028292,38.268554812991)) ;
#15420 = CARTESIAN_POINT('Ctrl Pts',(29.4,40.5221789060073,38.2759347604356)) ;
#15421 = CARTESIAN_POINT('Ctrl Pts',(29.4,40.5312329743323,38.2834075887112)) ;
#15422 = CARTESIAN_POINT('Ctrl Pts',(29.4,40.5402004635945,38.2909686978449)) ;
#15423 = CARTESIAN_POINT('Ctrl Pts',(29.4,40.5876132249798,38.3309456694014)) ;
#15424 = CARTESIAN_POINT('Ctrl Pts',(29.4,40.63264805134,38.373419504188)) ;
#15425 = CARTESIAN_POINT('Ctrl Pts',(29.4,40.6750367350389,38.4182522509551)) ;
#15426 = CARTESIAN_POINT('Ctrl Pts',(29.4,40.7166551699106,38.4622703375909)) ;
#15427 = CARTESIAN_POINT('Ctrl Pts',(29.4,40.7557232872012,38.5085630921309)) ;
#15428 = CARTESIAN_POINT('Ctrl Pts',(29.4,40.7919431689768,38.5570230298163)) ;
#15429 = CARTESIAN_POINT('Ctrl Pts',(29.4,40.8270103880344,38.6039407768387)) ;
#15430 = CARTESIAN_POINT('Ctrl Pts',(29.4,40.8594080675513,38.6528905689044)) ;
#15431 = CARTESIAN_POINT('Ctrl Pts',(29.4,40.8888183567986,38.703787175567)) ;
#15432 = CARTESIAN_POINT('Ctrl Pts',(29.4,40.8954530221445,38.7152689379396)) ;
#15433 = CARTESIAN_POINT('Ctrl Pts',(29.4,40.901935450219,38.7268498061172)) ;
#15434 = CARTESIAN_POINT('Ctrl Pts',(29.4,40.9082616204538,38.7385288450808)) ;
#15435 = CARTESIAN_POINT('Origin',(29.4,39.642135623731,39.642135623731)) ;
#15436 = CARTESIAN_POINT('Origin',(29.4,39.642135623731,39.642135623731)) ;
#15437 = CARTESIAN_POINT('Origin',(30.6940562256037,39.642135623731,39.642135623731)) ;
#15438 = CARTESIAN_POINT('Ctrl Pts',(29.4,40.9082616204539,38.7385288450808)) ;
#15439 = CARTESIAN_POINT('Ctrl Pts',(29.3630617283633,40.6086643314031,38.3187357169443)) ;
#15440 = CARTESIAN_POINT('Ctrl Pts',(29.2891851850898,39.5640416497925,37.8078105578506)) ;
#15441 = CARTESIAN_POINT('Ctrl Pts',(29.1783703701797,38.0585610812911,38.709446862677)) ;
#15442 = CARTESIAN_POINT('Ctrl Pts',(29.0675555552696,37.9986782664391,40.4614642406582)) ;
#15443 = CARTESIAN_POINT('Ctrl Pts',(28.9894508404109,39.0097624153104,41.1701268863298)) ;
#15444 = CARTESIAN_POINT('Ctrl Pts',(28.948284397189,39.5822413804429,41.1997935373523)) ;
#15445 = CARTESIAN_POINT('Ctrl Pts',(28.9440562256037,39.6410873345839,41.199362363652)) ;
#15446 = CARTESIAN_POINT('Ctrl Pts',(29.6300740822721,41.2326275540406,38.5070358837873)) ;
#15447 = CARTESIAN_POINT('Ctrl Pts',(29.5931358106354,40.8562771182931,37.9796969108663)) ;
#15448 = CARTESIAN_POINT('Ctrl Pts',(29.5192592673619,39.5440349325862,37.3378789996678)) ;
#15449 = CARTESIAN_POINT('Ctrl Pts',(29.4084444524518,37.6528687282456,38.4705034545895)) ;
#15450 = CARTESIAN_POINT('Ctrl Pts',(29.2976296375417,37.5776446715302,40.6713661717707)) ;
#15451 = CARTESIAN_POINT('Ctrl Pts',(29.1868148226315,39.3796763444381,41.9343990601139)) ;
#15452 = CARTESIAN_POINT('Ctrl Pts',(29.0760000077213,41.4218307707905,41.1108446083453)) ;
#15453 = CARTESIAN_POINT('Ctrl Pts',(28.9651851928113,41.8430894430381,38.9499197708456)) ;
#15454 = CARTESIAN_POINT('Ctrl Pts',(28.8543703779011,40.2607974022739,37.4193154134393)) ;
#15455 = CARTESIAN_POINT('Ctrl Pts',(28.743555562991,38.1151025245061,37.9124137447615)) ;
#15456 = CARTESIAN_POINT('Ctrl Pts',(28.6327407480808,37.3597577725899,39.9803498740405)) ;
#15457 = CARTESIAN_POINT('Ctrl Pts',(28.5219259331707,38.6823515624876,41.7403489526177)) ;
#15458 = CARTESIAN_POINT('Ctrl Pts',(28.4111111182605,40.8787925380227,41.5900502200798)) ;
#15459 = CARTESIAN_POINT('Ctrl Pts',(28.3002963033504,41.949318515855,39.6662829548393)) ;
#15460 = CARTESIAN_POINT('Ctrl Pts',(28.1894814884402,40.9192902716771,37.7205324493354)) ;
#15461 = CARTESIAN_POINT('Ctrl Pts',(28.0786666735301,38.7264830396968,37.5242915968402)) ;
#15462 = CARTESIAN_POINT('Ctrl Pts',(27.96785185862,37.3673265716251,39.2562276850161)) ;
#15463 = CARTESIAN_POINT('Ctrl Pts',(27.8570370437098,38.0792538124217,41.3395108148721)) ;
#15464 = CARTESIAN_POINT('Ctrl Pts',(27.7462222287997,40.2140963595073,41.8774304493772)) ;
#15465 = CARTESIAN_POINT('Ctrl Pts',(27.6354074138895,41.8282010360107,40.3802412053737)) ;
#15466 = CARTESIAN_POINT('Ctrl Pts',(27.5245925989794,41.4520175361157,38.2110488252218)) ;
#15467 = CARTESIAN_POINT('Ctrl Pts',(27.4137777840693,39.428039436314,37.3447795853464)) ;
#15468 = CARTESIAN_POINT('Ctrl Pts',(27.3029629691591,37.5989837588974,38.5701223869998)) ;
#15469 = CARTESIAN_POINT('Ctrl Pts',(27.192148154249,37.6301016629904,40.7714722784283)) ;
#15470 = CARTESIAN_POINT('Ctrl Pts',(27.0813333393388,39.4930620800583,41.9446253661672)) ;
#15471 = CARTESIAN_POINT('Ctrl Pts',(26.9705185244287,41.491745479404,41.0214924720458)) ;
#15472 = CARTESIAN_POINT('Ctrl Pts',(26.8597037095186,41.8064642830042,38.842533604026)) ;
#15473 = CARTESIAN_POINT('Ctrl Pts',(26.7488888946084,40.1506849147227,37.3915669059767)) ;
#15474 = CARTESIAN_POINT('Ctrl Pts',(26.6380740796983,38.0319003355603,37.9896150486028)) ;
#15475 = CARTESIAN_POINT('Ctrl Pts',(26.5272592647882,37.3791434212889,40.0921892054684)) ;
#15476 = CARTESIAN_POINT('Ctrl Pts',(26.416444449878,38.7867122240252,41.7850151681516)) ;
#15477 = CARTESIAN_POINT('Ctrl Pts',(26.3056296349679,40.9730953891353,41.5268711588974)) ;
#15478 = CARTESIAN_POINT('Ctrl Pts',(26.1948148200577,41.9477153719108,39.5527826189801)) ;
#15479 = CARTESIAN_POINT('Ctrl Pts',(26.0840000051476,40.8232360990565,37.6600449088926)) ;
#15480 = CARTESIAN_POINT('Ctrl Pts',(25.9731851902374,38.6234320058325,37.571888084536)) ;
#15481 = CARTESIAN_POINT('Ctrl Pts',(25.8623703753273,37.3510996288709,39.368573921512)) ;
#15482 = CARTESIAN_POINT('Ctrl Pts',(25.7515555604171,38.1646252471535,41.4143221324735)) ;
#15483 = CARTESIAN_POINT('Ctrl Pts',(25.640740745507,40.3233400457684,41.8465953013074)) ;
#15484 = CARTESIAN_POINT('Ctrl Pts',(25.5299259305969,41.8618569543069,40.2718332886862)) ;
#15485 = CARTESIAN_POINT('Ctrl Pts',(25.4191111156868,41.3794438141769,38.1237673594179)) ;
#15486 = CARTESIAN_POINT('Ctrl Pts',(25.3082963007766,39.3153103573985,37.3580893939119)) ;
#15487 = CARTESIAN_POINT('Ctrl Pts',(25.1974814858665,37.5487327209373,38.6719056400471)) ;
#15488 = CARTESIAN_POINT('Ctrl Pts',(25.0866666709563,37.6880793876533,40.869061114912)) ;
#15489 = CARTESIAN_POINT('Ctrl Pts',(24.9758518560462,39.6064831413471,41.9491706982723)) ;
#15490 = CARTESIAN_POINT('Ctrl Pts',(24.865037041136,41.5573464528993,40.9288560341155)) ;
#15491 = CARTESIAN_POINT('Ctrl Pts',(24.7542222262259,41.764519211549,38.7370556047135)) ;
#15492 = CARTESIAN_POINT('Ctrl Pts',(24.6434074113157,40.0393824012721,37.3692790659172)) ;
#15493 = CARTESIAN_POINT('Ctrl Pts',(24.5325925964056,37.95257498919,38.0708091786937)) ;
#15494 = CARTESIAN_POINT('Ctrl Pts',(24.4217777814955,37.4040164592344,40.2029426673539)) ;
#15495 = CARTESIAN_POINT('Ctrl Pts',(24.3109629665854,38.8931381595526,41.8244932326755)) ;
#15496 = CARTESIAN_POINT('Ctrl Pts',(24.2001481516752,41.0641794598153,41.4591312932135)) ;
#15497 = CARTESIAN_POINT('Ctrl Pts',(24.0893333367651,41.9405307108,39.4394981188101)) ;
#15498 = CARTESIAN_POINT('Ctrl Pts',(23.9785185218549,40.7243239315548,37.6043548698045)) ;
#15499 = CARTESIAN_POINT('Ctrl Pts',(23.8677037069448,38.5228462358779,37.6244951203447)) ;
#15500 = CARTESIAN_POINT('Ctrl Pts',(23.7568888920346,37.340417880274,39.4815823175755)) ;
#15501 = CARTESIAN_POINT('Ctrl Pts',(23.6460740771245,38.2535726445995,41.4848441703134)) ;
#15502 = CARTESIAN_POINT('Ctrl Pts',(23.5352592622144,40.4309350418146,41.8104246756579)) ;
#15503 = CARTESIAN_POINT('Ctrl Pts',(23.4244444473042,41.8901404233572,40.1619012973779)) ;
#15504 = CARTESIAN_POINT('Ctrl Pts',(23.3136296323941,41.302665265992,38.0401608293496)) ;
#15505 = CARTESIAN_POINT('Ctrl Pts',(23.2028148174839,39.2033722941205,37.3769273164583)) ;
#15506 = CARTESIAN_POINT('Ctrl Pts',(23.0920000025738,37.5035483839543,38.7760371579915)) ;
#15507 = CARTESIAN_POINT('Ctrl Pts',(22.9811851876637,37.750786546316,40.9636804024138)) ;
#15508 = CARTESIAN_POINT('Ctrl Pts',(22.8703703727535,39.7199904936858,41.948132274746)) ;
#15509 = CARTESIAN_POINT('Ctrl Pts',(22.7595555578434,41.6183120087299,40.8331053246757)) ;
#15510 = CARTESIAN_POINT('Ctrl Pts',(22.6487407429333,41.7174372998317,38.6337681864242)) ;
#15511 = CARTESIAN_POINT('Ctrl Pts',(22.5379259280231,39.9271184237843,37.3524922579445)) ;
#15512 = CARTESIAN_POINT('Ctrl Pts',(22.427111113113,37.877338916748,38.1558064187693)) ;
#15513 = CARTESIAN_POINT('Ctrl Pts',(22.3162962982028,37.4343064513157,40.3123387944194)) ;
#15514 = CARTESIAN_POINT('Ctrl Pts',(22.2054814832926,39.0013769132445,41.8586893083008)) ;
#15515 = CARTESIAN_POINT('Ctrl Pts',(22.0946666683825,41.1518217199103,41.3869937060463)) ;
#15516 = CARTESIAN_POINT('Ctrl Pts',(21.9838518534724,41.9277832329101,39.3267040979053)) ;
#15517 = CARTESIAN_POINT('Ctrl Pts',(21.8730370385623,40.622792470112,37.5535968414076)) ;
#15518 = CARTESIAN_POINT('Ctrl Pts',(21.7622222236521,38.4249696113942,37.6819856143904)) ;
#15519 = CARTESIAN_POINT('Ctrl Pts',(21.651407408742,37.3353067973815,39.5949790461577)) ;
#15520 = CARTESIAN_POINT('Ctrl Pts',(21.5405925938318,38.3458812452266,41.5509067836203)) ;
#15521 = CARTESIAN_POINT('Ctrl Pts',(21.4297777789217,40.5366200128897,41.7690050764386)) ;
#15522 = CARTESIAN_POINT('Ctrl Pts',(21.3189629640115,41.9129847670933,40.0507133598168)) ;
#15523 = CARTESIAN_POINT('Ctrl Pts',(21.2081481491014,41.2218641967656,37.960427488152)) ;
#15524 = CARTESIAN_POINT('Ctrl Pts',(21.0973333341913,39.0925031947873,37.4012559465627)) ;
#15525 = CARTESIAN_POINT('Ctrl Pts',(20.9865185192811,37.4635260875702,38.8822485573436)) ;
#15526 = CARTESIAN_POINT('Ctrl Pts',(20.875703704371,37.8180993714967,41.0551337957205)) ;
#15527 = CARTESIAN_POINT('Ctrl Pts',(20.7648888894609,39.8332534757639,41.9414473616958)) ;
#15528 = CARTESIAN_POINT('Ctrl Pts',(20.6540740745507,41.6746063303626,40.7346024308416)) ;
#15529 = CARTESIAN_POINT('Ctrl Pts',(20.5432592596406,41.6651092776103,38.5326609143414)) ;
#15530 = CARTESIAN_POINT('Ctrl Pts',(20.4324444447304,39.814610819179,37.3417681053347)) ;
#15531 = CARTESIAN_POINT('Ctrl Pts',(20.3216296298203,37.8054802267138,38.2433498381838)) ;
#15532 = CARTESIAN_POINT('Ctrl Pts',(20.2108148149101,37.4717648473903,40.4223362571249)) ;
#15533 = CARTESIAN_POINT('Ctrl Pts',(20.1369382716367,38.561997188093,41.394603313221)) ;
#15534 = CARTESIAN_POINT('Ctrl Pts',(20.1,39.1924719723276,41.5436925123374)) ;
#15535 = CARTESIAN_POINT('Ctrl Pts',(29.5533827215147,41.1245055761783,38.5842002042185)) ;
#15536 = CARTESIAN_POINT('Ctrl Pts',(29.516444449878,40.7737395226631,38.0927098462256)) ;
#15537 = CARTESIAN_POINT('Ctrl Pts',(29.4425679066046,39.5507038383217,37.4945228523954)) ;
#15538 = CARTESIAN_POINT('Ctrl Pts',(29.3317530916944,37.7880995125941,38.5501512572853)) ;
#15539 = CARTESIAN_POINT('Ctrl Pts',(29.2209382767843,37.7179892031665,40.6013988613999)) ;
#15540 = CARTESIAN_POINT('Ctrl Pts',(29.1101234618742,39.3975183817629,41.7785705068217)) ;
#15541 = CARTESIAN_POINT('Ctrl Pts',(28.999308646964,41.3008467182311,41.0110014608924)) ;
#15542 = CARTESIAN_POINT('Ctrl Pts',(28.8884938320539,41.6934681368296,38.9969767509505)) ;
#15543 = CARTESIAN_POINT('Ctrl Pts',(28.7776790171438,40.2187406437018,37.5704232015323)) ;
#15544 = CARTESIAN_POINT('Ctrl Pts',(28.6668642022336,38.2189105576076,38.0300006039852)) ;
#15545 = CARTESIAN_POINT('Ctrl Pts',(28.5560493873235,37.5149143017061,39.9573579977613)) ;
#15546 = CARTESIAN_POINT('Ctrl Pts',(28.4452345724133,38.7475978859959,41.5977119666809)) ;
#15547 = CARTESIAN_POINT('Ctrl Pts',(28.3344197575032,40.7947243393968,41.4576305737739)) ;
#15548 = CARTESIAN_POINT('Ctrl Pts',(28.223604942593,41.7924757348056,39.6646414141626)) ;
#15549 = CARTESIAN_POINT('Ctrl Pts',(28.1127901276829,40.8324690285507,37.8511634396112)) ;
#15550 = CARTESIAN_POINT('Ctrl Pts',(28.0019753127728,38.7887292960491,37.6682630817799)) ;
#15551 = CARTESIAN_POINT('Ctrl Pts',(27.8911604978626,37.521968572182,39.2824617883217)) ;
#15552 = CARTESIAN_POINT('Ctrl Pts',(27.7803456829525,38.1854988485539,41.2241228903294)) ;
#15553 = CARTESIAN_POINT('Ctrl Pts',(27.6695308680424,40.1752143477012,41.7254746342936)) ;
#15554 = CARTESIAN_POINT('Ctrl Pts',(27.5587160531322,41.6795918468614,40.3300646318007)) ;
#15555 = CARTESIAN_POINT('Ctrl Pts',(27.4479012382221,41.328981380864,38.308334408505)) ;
#15556 = CARTESIAN_POINT('Ctrl Pts',(27.3370864233119,39.4425937404228,37.5009543347999)) ;
#15557 = CARTESIAN_POINT('Ctrl Pts',(27.2262716084018,37.7378776548606,38.6429980735978)) ;
#15558 = CARTESIAN_POINT('Ctrl Pts',(27.1154567934916,37.7668801572509,40.6946997337513)) ;
#15559 = CARTESIAN_POINT('Ctrl Pts',(27.0046419785815,39.503196131091,41.7881016264263)) ;
#15560 = CARTESIAN_POINT('Ctrl Pts',(26.8938271636713,41.3660086101638,40.9277235017194)) ;
#15561 = CARTESIAN_POINT('Ctrl Pts',(26.7830123487612,41.6593327629223,38.8968907184669)) ;
#15562 = CARTESIAN_POINT('Ctrl Pts',(26.6721975338511,40.1161136263466,37.5445610434767)) ;
#15563 = CARTESIAN_POINT('Ctrl Pts',(26.5613827189409,38.1413644710663,38.1019537468609)) ;
#15564 = CARTESIAN_POINT('Ctrl Pts',(26.4505679040308,37.532982109906,40.0615944677811)) ;
#15565 = CARTESIAN_POINT('Ctrl Pts',(26.3397530891206,38.8448640876866,41.6393417634346)) ;
#15566 = CARTESIAN_POINT('Ctrl Pts',(26.2289382742105,40.8826164627426,41.3987464385351)) ;
#15567 = CARTESIAN_POINT('Ctrl Pts',(26.1181234593003,41.7909815729259,39.5588568551441)) ;
#15568 = CARTESIAN_POINT('Ctrl Pts',(26.0073086443903,40.7429446389034,37.7947878549628)) ;
#15569 = CARTESIAN_POINT('Ctrl Pts',(25.8964938294801,38.6926836932656,37.7126239501739)) ;
#15570 = CARTESIAN_POINT('Ctrl Pts',(25.78567901457,37.5068447404287,39.3871707038959)) ;
#15571 = CARTESIAN_POINT('Ctrl Pts',(25.6748641996598,38.2650667150938,41.2938485187352)) ;
#15572 = CARTESIAN_POINT('Ctrl Pts',(25.5640493847497,40.2770316250618,41.6967356661122)) ;
#15573 = CARTESIAN_POINT('Ctrl Pts',(25.4532345698395,41.7109598287124,40.2290263082214)) ;
#15574 = CARTESIAN_POINT('Ctrl Pts',(25.3424197549294,41.2613412358943,38.2269863552092)) ;
#15575 = CARTESIAN_POINT('Ctrl Pts',(25.2316049400193,39.3375280081377,37.5133593397636)) ;
#15576 = CARTESIAN_POINT('Ctrl Pts',(25.1207901251091,37.6910426930908,38.7378620795726)) ;
#15577 = CARTESIAN_POINT('Ctrl Pts',(25.009975310199,37.820916543927,40.7856544604875)) ;
#15578 = CARTESIAN_POINT('Ctrl Pts',(24.8991604952888,39.6089068046413,41.7923379658934)) ;
#15579 = CARTESIAN_POINT('Ctrl Pts',(24.7883456803787,41.4271500156042,40.8413845084351)) ;
#15580 = CARTESIAN_POINT('Ctrl Pts',(24.6775308654685,41.6202391262972,38.7985831358596)) ;
#15581 = CARTESIAN_POINT('Ctrl Pts',(24.5667160505584,40.0123774813045,37.5237883354991)) ;
#15582 = CARTESIAN_POINT('Ctrl Pts',(24.4559012356483,38.0674316785221,38.177628282813)) ;
#15583 = CARTESIAN_POINT('Ctrl Pts',(24.3450864207381,37.5561642734705,40.1648188858998)) ;
#15584 = CARTESIAN_POINT('Ctrl Pts',(24.234271605828,38.9440551656044,41.6761361007812)) ;
#15585 = CARTESIAN_POINT('Ctrl Pts',(24.1234567909178,40.9675086190306,41.3356115432495)) ;
#15586 = CARTESIAN_POINT('Ctrl Pts',(24.0126419760077,41.7842853265972,39.4532734592589)) ;
#15587 = CARTESIAN_POINT('Ctrl Pts',(23.9018271610975,40.6507565414716,37.7428836365121)) ;
#15588 = CARTESIAN_POINT('Ctrl Pts',(23.7910123461874,38.5989357652295,37.7616547485602)) ;
#15589 = CARTESIAN_POINT('Ctrl Pts',(23.6801975312773,37.496889139361,39.4924967652901)) ;
#15590 = CARTESIAN_POINT('Ctrl Pts',(23.5693827163671,38.3479674496463,41.3595764535251)) ;
#15591 = CARTESIAN_POINT('Ctrl Pts',(23.458567901457,40.377312290517,41.6630239272456)) ;
#15592 = CARTESIAN_POINT('Ctrl Pts',(23.3477530865469,41.7373205815539,40.1265675169364)) ;
#15593 = CARTESIAN_POINT('Ctrl Pts',(23.2369382716367,41.1897821096561,38.1490634147404)) ;
#15594 = CARTESIAN_POINT('Ctrl Pts',(23.1261234567266,39.2331995180799,37.5309166563505)) ;
#15595 = CARTESIAN_POINT('Ctrl Pts',(23.0153086418164,37.6489299968938,38.8349147149)) ;
#15596 = CARTESIAN_POINT('Ctrl Pts',(22.9044938269063,37.8793608566794,40.87384150881)) ;
#15597 = CARTESIAN_POINT('Ctrl Pts',(22.7936790119962,39.7146979031575,41.7913701346181)) ;
#15598 = CARTESIAN_POINT('Ctrl Pts',(22.682864197086,41.4839711200533,40.7521429524774)) ;
#15599 = CARTESIAN_POINT('Ctrl Pts',(22.5720493821759,41.5763578528978,38.7023172181142)) ;
#15600 = CARTESIAN_POINT('Ctrl Pts',(22.4612345672657,39.9077452327537,37.5081426982832)) ;
#15601 = CARTESIAN_POINT('Ctrl Pts',(22.3504197523556,37.9973101701995,38.2568473925287)) ;
#15602 = CARTESIAN_POINT('Ctrl Pts',(22.2396049374455,37.5843951454828,40.2667782411066)) ;
#15603 = CARTESIAN_POINT('Ctrl Pts',(22.1287901225353,39.0449358259243,41.708007519952)) ;
#15604 = CARTESIAN_POINT('Ctrl Pts',(22.0179753076252,41.0491929397452,41.2683778845173)) ;
#15605 = CARTESIAN_POINT('Ctrl Pts',(21.907160492715,41.7724044249507,39.3481471997548)) ;
#15606 = CARTESIAN_POINT('Ctrl Pts',(21.7963456778049,40.5561272102548,37.6955761496225)) ;
#15607 = CARTESIAN_POINT('Ctrl Pts',(21.6855308628947,38.5077128143823,37.8152370266596)) ;
#15608 = CARTESIAN_POINT('Ctrl Pts',(21.5747160479846,37.4921255089646,39.5981847602763)) ;
#15609 = CARTESIAN_POINT('Ctrl Pts',(21.4639012330745,38.4340008920765,41.421148116405)) ;
#15610 = CARTESIAN_POINT('Ctrl Pts',(21.3530864181644,40.4758127749028,41.6244200411428)) ;
#15611 = CARTESIAN_POINT('Ctrl Pts',(21.2422716032542,41.7586119619704,40.0229381588904)) ;
#15612 = CARTESIAN_POINT('Ctrl Pts',(21.1314567883441,41.1144739142077,38.0747503629435)) ;
#15613 = CARTESIAN_POINT('Ctrl Pts',(21.0206419734339,39.1298673235717,37.5535914210342)) ;
#15614 = CARTESIAN_POINT('Ctrl Pts',(20.9098271585238,37.6116284246838,38.9339058408569)) ;
#15615 = CARTESIAN_POINT('Ctrl Pts',(20.7990123436136,37.9420977417654,40.9590778810945)) ;
#15616 = CARTESIAN_POINT('Ctrl Pts',(20.6881975287035,39.8202612437552,41.7851396633712)) ;
#15617 = CARTESIAN_POINT('Ctrl Pts',(20.5773827137933,41.5364385417934,40.6603363062026)) ;
#15618 = CARTESIAN_POINT('Ctrl Pts',(20.4665678988832,41.5275871006961,38.6080832397749)) ;
#15619 = CARTESIAN_POINT('Ctrl Pts',(20.355753083973,39.8028859189084,37.4981475758365)) ;
#15620 = CARTESIAN_POINT('Ctrl Pts',(20.2449382690629,37.9303364491143,38.3384395917731)) ;
#15621 = CARTESIAN_POINT('Ctrl Pts',(20.1341234541528,37.6193071118685,40.3692980530295)) ;
#15622 = CARTESIAN_POINT('Ctrl Pts',(20.0602469108794,38.6354252274314,41.2754701889866)) ;
#15623 = CARTESIAN_POINT('Ctrl Pts',(20.0233086392427,39.2230402024682,41.41442427281)) ;
#15624 = CARTESIAN_POINT('Ctrl Pts',(29.4766913607574,41.0163835983161,38.6613645246497)) ;
#15625 = CARTESIAN_POINT('Ctrl Pts',(29.4397530891207,40.6912019270331,38.205722781585)) ;
#15626 = CARTESIAN_POINT('Ctrl Pts',(29.3658765458472,39.5573727440571,37.6511667051229)) ;
#15627 = CARTESIAN_POINT('Ctrl Pts',(29.2550617309371,37.9233302969426,38.6297990599812)) ;
#15628 = CARTESIAN_POINT('Ctrl Pts',(29.144246916027,37.8583337348028,40.531431551029)) ;
#15629 = CARTESIAN_POINT('Ctrl Pts',(29.0334321011168,39.4153604190877,41.6227419535296)) ;
#15630 = CARTESIAN_POINT('Ctrl Pts',(28.9226172862066,41.1798626656718,40.9111583134396)) ;
#15631 = CARTESIAN_POINT('Ctrl Pts',(28.8118024712965,41.5438468306211,39.0440337310553)) ;
#15632 = CARTESIAN_POINT('Ctrl Pts',(28.7009876563864,40.1766838851298,37.7215309896254)) ;
#15633 = CARTESIAN_POINT('Ctrl Pts',(28.5901728414763,38.3227185907092,38.1475874632089)) ;
#15634 = CARTESIAN_POINT('Ctrl Pts',(28.4793580265661,37.6700708308224,39.9343661214822)) ;
#15635 = CARTESIAN_POINT('Ctrl Pts',(28.368543211656,38.8128442095042,41.4550749807441)) ;
#15636 = CARTESIAN_POINT('Ctrl Pts',(28.2577283967458,40.7106561407708,41.325210927468)) ;
#15637 = CARTESIAN_POINT('Ctrl Pts',(28.1469135818357,41.6356329537562,39.6629998734859)) ;
#15638 = CARTESIAN_POINT('Ctrl Pts',(28.0360987669255,40.7456477854244,37.981794429887)) ;
#15639 = CARTESIAN_POINT('Ctrl Pts',(27.9252839520154,38.8509755524015,37.8122345667194)) ;
#15640 = CARTESIAN_POINT('Ctrl Pts',(27.8144691371052,37.6766105727388,39.3086958916275)) ;
#15641 = CARTESIAN_POINT('Ctrl Pts',(27.7036543221951,38.291743884686,41.1087349657866)) ;
#15642 = CARTESIAN_POINT('Ctrl Pts',(27.592839507285,40.1363323358952,41.57351881921)) ;
#15643 = CARTESIAN_POINT('Ctrl Pts',(27.4820246923748,41.5309826577121,40.2798880582278)) ;
#15644 = CARTESIAN_POINT('Ctrl Pts',(27.3712098774647,41.2059452256123,38.4056199917881)) ;
#15645 = CARTESIAN_POINT('Ctrl Pts',(27.2603950625546,39.4571480445315,37.6571290842533)) ;
#15646 = CARTESIAN_POINT('Ctrl Pts',(27.1495802476444,37.8767715508238,38.7158737601958)) ;
#15647 = CARTESIAN_POINT('Ctrl Pts',(27.0387654327343,37.9036586515114,40.6179271890742)) ;
#15648 = CARTESIAN_POINT('Ctrl Pts',(26.9279506178242,39.5133301821237,41.6315778866856)) ;
#15649 = CARTESIAN_POINT('Ctrl Pts',(26.817135802914,41.2402717409236,40.8339545313929)) ;
#15650 = CARTESIAN_POINT('Ctrl Pts',(26.7063209880039,41.5122012428404,38.9512478329077)) ;
#15651 = CARTESIAN_POINT('Ctrl Pts',(26.5955061730937,40.0815423379706,37.6975551809767)) ;
#15652 = CARTESIAN_POINT('Ctrl Pts',(26.4846913581836,38.2508286065723,38.2142924451189)) ;
#15653 = CARTESIAN_POINT('Ctrl Pts',(26.3738765432735,37.686820798523,40.030999730094)) ;
#15654 = CARTESIAN_POINT('Ctrl Pts',(26.2630617283633,38.9030159513479,41.4936683587175)) ;
#15655 = CARTESIAN_POINT('Ctrl Pts',(26.1522469134532,40.7921375363501,41.2706217181728)) ;
#15656 = CARTESIAN_POINT('Ctrl Pts',(26.041432098543,41.6342477739409,39.564931091308)) ;
#15657 = CARTESIAN_POINT('Ctrl Pts',(25.9306172836329,40.6626531787504,37.9295308010329)) ;
#15658 = CARTESIAN_POINT('Ctrl Pts',(25.8198024687227,38.7619353806986,37.8533598158118)) ;
#15659 = CARTESIAN_POINT('Ctrl Pts',(25.7089876538126,37.6625898519865,39.4057674862797)) ;
#15660 = CARTESIAN_POINT('Ctrl Pts',(25.5981728389024,38.3655081830341,41.173374904997)) ;
#15661 = CARTESIAN_POINT('Ctrl Pts',(25.4873580239923,40.2307232043552,41.546876030917)) ;
#15662 = CARTESIAN_POINT('Ctrl Pts',(25.3765432090821,41.5600627031181,40.1862193277566)) ;
#15663 = CARTESIAN_POINT('Ctrl Pts',(25.2657283941721,41.1432386576117,38.3302053510005)) ;
#15664 = CARTESIAN_POINT('Ctrl Pts',(25.1549135792619,39.359745658877,37.6686292856154)) ;
#15665 = CARTESIAN_POINT('Ctrl Pts',(25.0440987643518,37.8333526652442,38.803818519098)) ;
#15666 = CARTESIAN_POINT('Ctrl Pts',(24.9332839494416,37.9537537002008,40.7022478060632)) ;
#15667 = CARTESIAN_POINT('Ctrl Pts',(24.8224691345315,39.6113304679353,41.6355052335146)) ;
#15668 = CARTESIAN_POINT('Ctrl Pts',(24.7116543196213,41.2969535783092,40.7539129827547)) ;
#15669 = CARTESIAN_POINT('Ctrl Pts',(24.6008395047112,41.4759590410456,38.8601106670057)) ;
#15670 = CARTESIAN_POINT('Ctrl Pts',(24.490024689801,39.9853725613369,37.6782976050809)) ;
#15671 = CARTESIAN_POINT('Ctrl Pts',(24.3792098748909,38.1822883678541,38.2844473869324)) ;
#15672 = CARTESIAN_POINT('Ctrl Pts',(24.2683950599807,37.7083120877066,40.1266951044458)) ;
#15673 = CARTESIAN_POINT('Ctrl Pts',(24.1575802450706,38.994972171656,41.5277789688869)) ;
#15674 = CARTESIAN_POINT('Ctrl Pts',(24.0467654301605,40.870837778246,41.2120917932856)) ;
#15675 = CARTESIAN_POINT('Ctrl Pts',(23.9359506152503,41.6280399423943,39.4670487997076)) ;
#15676 = CARTESIAN_POINT('Ctrl Pts',(23.8251358003402,40.5771891513884,37.8814124032197)) ;
#15677 = CARTESIAN_POINT('Ctrl Pts',(23.71432098543,38.6750252945812,37.8988143767757)) ;
#15678 = CARTESIAN_POINT('Ctrl Pts',(23.6035061705199,37.6533603984479,39.5034112130047)) ;
#15679 = CARTESIAN_POINT('Ctrl Pts',(23.4926913556098,38.4423622546929,41.2343087367368)) ;
#15680 = CARTESIAN_POINT('Ctrl Pts',(23.3818765406997,40.3236895392195,41.5156231788333)) ;
#15681 = CARTESIAN_POINT('Ctrl Pts',(23.2710617257895,41.5845007397505,40.0912337364948)) ;
#15682 = CARTESIAN_POINT('Ctrl Pts',(23.1602469108794,41.0768989533203,38.2579660001312)) ;
#15683 = CARTESIAN_POINT('Ctrl Pts',(23.0494320959692,39.2630267420392,37.6849059962426)) ;
#15684 = CARTESIAN_POINT('Ctrl Pts',(22.9386172810591,37.7943116098333,38.8937922718084)) ;
#15685 = CARTESIAN_POINT('Ctrl Pts',(22.827802466149,38.0079351670427,40.7840026152063)) ;
#15686 = CARTESIAN_POINT('Ctrl Pts',(22.7169876512388,39.7094053126292,41.6346079944903)) ;
#15687 = CARTESIAN_POINT('Ctrl Pts',(22.6061728363287,41.3496302313767,40.6711805802791)) ;
#15688 = CARTESIAN_POINT('Ctrl Pts',(22.4953580214185,41.435278405964,38.7708662498041)) ;
#15689 = CARTESIAN_POINT('Ctrl Pts',(22.3845432065084,39.8883720417231,37.663793138622)) ;
#15690 = CARTESIAN_POINT('Ctrl Pts',(22.2737283915983,38.117281423651,38.357888366288)) ;
#15691 = CARTESIAN_POINT('Ctrl Pts',(22.1629135766881,37.7344838396499,40.2212176877939)) ;
#15692 = CARTESIAN_POINT('Ctrl Pts',(22.0520987617779,39.088494738604,41.5573257316031)) ;
#15693 = CARTESIAN_POINT('Ctrl Pts',(21.9412839468678,40.9465641595803,41.1497620629884)) ;
#15694 = CARTESIAN_POINT('Ctrl Pts',(21.8304691319577,41.6170256169913,39.3695903016042)) ;
#15695 = CARTESIAN_POINT('Ctrl Pts',(21.7196543170475,40.4894619503976,37.8375554578374)) ;
#15696 = CARTESIAN_POINT('Ctrl Pts',(21.6088395021374,38.5904560173703,37.9484884389288)) ;
#15697 = CARTESIAN_POINT('Ctrl Pts',(21.4980246872273,37.6489442205477,39.6013904743948)) ;
#15698 = CARTESIAN_POINT('Ctrl Pts',(21.3872098723171,38.5221205389264,41.2913894491898)) ;
#15699 = CARTESIAN_POINT('Ctrl Pts',(21.276395057407,40.4150055369158,41.479835005847)) ;
#15700 = CARTESIAN_POINT('Ctrl Pts',(21.1655802424968,41.6042391568477,39.9951629579641)) ;
#15701 = CARTESIAN_POINT('Ctrl Pts',(21.0547654275867,41.0070836316498,38.1890732377351)) ;
#15702 = CARTESIAN_POINT('Ctrl Pts',(20.9439506126765,39.167231452356,37.7059268955056)) ;
#15703 = CARTESIAN_POINT('Ctrl Pts',(20.8331357977664,37.7597307617974,38.9855631243703)) ;
#15704 = CARTESIAN_POINT('Ctrl Pts',(20.7223209828563,38.0660961120341,40.8630219664685)) ;
#15705 = CARTESIAN_POINT('Ctrl Pts',(20.6115061679461,39.8072690117465,41.6288319650465)) ;
#15706 = CARTESIAN_POINT('Ctrl Pts',(20.500691353036,41.3982707532242,40.5860701815637)) ;
#15707 = CARTESIAN_POINT('Ctrl Pts',(20.3898765381259,41.3900649237819,38.6835055652085)) ;
#15708 = CARTESIAN_POINT('Ctrl Pts',(20.2790617232157,39.7911610186378,37.6545270463381)) ;
#15709 = CARTESIAN_POINT('Ctrl Pts',(20.1682469083056,38.0551926715147,38.4335293453624)) ;
#15710 = CARTESIAN_POINT('Ctrl Pts',(20.0574320933955,37.7668493763468,40.3162598489341)) ;
#15711 = CARTESIAN_POINT('Ctrl Pts',(19.983555550122,38.7088532667698,41.1563370647523)) ;
#15712 = CARTESIAN_POINT('Ctrl Pts',(19.9466172784853,39.2536084326088,41.2851560332826)) ;
#15713 = CARTESIAN_POINT('Ctrl Pts',(29.4,40.9082616204539,38.7385288450808)) ;
#15714 = CARTESIAN_POINT('Ctrl Pts',(29.3630617283633,40.6086643314031,38.3187357169443)) ;
#15715 = CARTESIAN_POINT('Ctrl Pts',(29.2891851850898,39.5640416497925,37.8078105578506)) ;
#15716 = CARTESIAN_POINT('Ctrl Pts',(29.1783703701797,38.0585610812911,38.709446862677)) ;
#15717 = CARTESIAN_POINT('Ctrl Pts',(29.0675555552696,37.9986782664391,40.4614642406582)) ;
#15718 = CARTESIAN_POINT('Ctrl Pts',(28.9567407403595,39.4332024564126,41.4669134002374)) ;
#15719 = CARTESIAN_POINT('Ctrl Pts',(28.8459259254493,41.0588786131123,40.8113151659867)) ;
#15720 = CARTESIAN_POINT('Ctrl Pts',(28.7351111105392,41.3942255244127,39.0910907111602)) ;
#15721 = CARTESIAN_POINT('Ctrl Pts',(28.624296295629,40.1346271265577,37.8726387777184)) ;
#15722 = CARTESIAN_POINT('Ctrl Pts',(28.5134814807189,38.4265266238107,38.2651743224326)) ;
#15723 = CARTESIAN_POINT('Ctrl Pts',(28.4026666658087,37.8252273599387,39.911374245203)) ;
#15724 = CARTESIAN_POINT('Ctrl Pts',(28.2918518508986,38.8780905330125,41.3124379948074)) ;
#15725 = CARTESIAN_POINT('Ctrl Pts',(28.1810370359884,40.6265879421449,41.1927912811621)) ;
#15726 = CARTESIAN_POINT('Ctrl Pts',(28.0702222210783,41.4787901727068,39.6613583328092)) ;
#15727 = CARTESIAN_POINT('Ctrl Pts',(27.9594074061682,40.6588265422981,38.1124254201628)) ;
#15728 = CARTESIAN_POINT('Ctrl Pts',(27.848592591258,38.9132218087539,37.956206051659)) ;
#15729 = CARTESIAN_POINT('Ctrl Pts',(27.7377777763479,37.8312525732956,39.3349299949331)) ;
#15730 = CARTESIAN_POINT('Ctrl Pts',(27.6269629614378,38.3979889208182,40.9933470412438)) ;
#15731 = CARTESIAN_POINT('Ctrl Pts',(27.5161481465276,40.0974503240892,41.4215630041264)) ;
#15732 = CARTESIAN_POINT('Ctrl Pts',(27.4053333316175,41.3823734685628,40.2297114846548)) ;
#15733 = CARTESIAN_POINT('Ctrl Pts',(27.2945185167073,41.0829090703606,38.5029055750713)) ;
#15734 = CARTESIAN_POINT('Ctrl Pts',(27.1837037017972,39.4717023486403,37.8133038337068)) ;
#15735 = CARTESIAN_POINT('Ctrl Pts',(27.0728888868871,38.0156654467869,38.7887494467938)) ;
#15736 = CARTESIAN_POINT('Ctrl Pts',(26.9620740719769,38.0404371457719,40.5411546443971)) ;
#15737 = CARTESIAN_POINT('Ctrl Pts',(26.8512592570668,39.5234642331564,41.4750541469447)) ;
#15738 = CARTESIAN_POINT('Ctrl Pts',(26.7404444421566,41.1145348716835,40.7401855610665)) ;
#15739 = CARTESIAN_POINT('Ctrl Pts',(26.6296296272465,41.3650697227584,39.0056049473486)) ;
#15740 = CARTESIAN_POINT('Ctrl Pts',(26.5188148123364,40.0469710495945,37.8505493184767)) ;
#15741 = CARTESIAN_POINT('Ctrl Pts',(26.4079999974262,38.3602927420783,38.3266311433769)) ;
#15742 = CARTESIAN_POINT('Ctrl Pts',(26.2971851825161,37.8406594871401,40.0004049924068)) ;
#15743 = CARTESIAN_POINT('Ctrl Pts',(26.1863703676059,38.9611678150092,41.3479949540004)) ;
#15744 = CARTESIAN_POINT('Ctrl Pts',(26.0755555526958,40.7016586099574,41.1424969978105)) ;
#15745 = CARTESIAN_POINT('Ctrl Pts',(25.9647407377856,41.477513974956,39.571005327472)) ;
#15746 = CARTESIAN_POINT('Ctrl Pts',(25.8539259228755,40.5823617185973,38.064273747103)) ;
#15747 = CARTESIAN_POINT('Ctrl Pts',(25.7431111079654,38.8311870681316,37.9940956814497)) ;
#15748 = CARTESIAN_POINT('Ctrl Pts',(25.6322962930552,37.8183349635443,39.4243642686637)) ;
#15749 = CARTESIAN_POINT('Ctrl Pts',(25.5214814781451,38.4659496509744,41.0529012912587)) ;
#15750 = CARTESIAN_POINT('Ctrl Pts',(25.410666663235,40.1844147836487,41.3970163957218)) ;
#15751 = CARTESIAN_POINT('Ctrl Pts',(25.2998518483248,41.4091655775236,40.1434123472918)) ;
#15752 = CARTESIAN_POINT('Ctrl Pts',(25.1890370334147,41.0251360793291,38.4334243467918)) ;
#15753 = CARTESIAN_POINT('Ctrl Pts',(25.0782222185045,39.3819633096162,37.8238992314671)) ;
#15754 = CARTESIAN_POINT('Ctrl Pts',(24.9674074035944,37.9756626373976,38.8697749586234)) ;
#15755 = CARTESIAN_POINT('Ctrl Pts',(24.8565925886842,38.0865908564746,40.6188411516388)) ;
#15756 = CARTESIAN_POINT('Ctrl Pts',(24.7457777737741,39.6137541312294,41.4786725011358)) ;
#15757 = CARTESIAN_POINT('Ctrl Pts',(24.634962958864,41.1667571410141,40.6664414570744)) ;
#15758 = CARTESIAN_POINT('Ctrl Pts',(24.5241481439538,41.3316789557939,38.9216381981518)) ;
#15759 = CARTESIAN_POINT('Ctrl Pts',(24.4133333290437,39.9583676413693,37.8328068746627)) ;
#15760 = CARTESIAN_POINT('Ctrl Pts',(24.3025185141336,38.2971450571862,38.3912664910517)) ;
#15761 = CARTESIAN_POINT('Ctrl Pts',(24.1917036992234,37.8604599019426,40.0885713229918)) ;
#15762 = CARTESIAN_POINT('Ctrl Pts',(24.0808888843133,39.0458891777078,41.3794218369926)) ;
#15763 = CARTESIAN_POINT('Ctrl Pts',(23.9700740694031,40.7741669374613,41.0885720433216)) ;
#15764 = CARTESIAN_POINT('Ctrl Pts',(23.859259254493,41.4717945581916,39.4808241401565)) ;
#15765 = CARTESIAN_POINT('Ctrl Pts',(23.7484444395829,40.5036217613051,38.0199411699272)) ;
#15766 = CARTESIAN_POINT('Ctrl Pts',(23.6376296246727,38.7511148239329,38.0359740049913)) ;
#15767 = CARTESIAN_POINT('Ctrl Pts',(23.5268148097626,37.8098316575348,39.5143256607193)) ;
#15768 = CARTESIAN_POINT('Ctrl Pts',(23.4159999948524,38.5367570597397,41.1090410199485)) ;
#15769 = CARTESIAN_POINT('Ctrl Pts',(23.3051851799423,40.2700667879219,41.368222430421)) ;
#15770 = CARTESIAN_POINT('Ctrl Pts',(23.1943703650321,41.4316808979472,40.0558999560533)) ;
#15771 = CARTESIAN_POINT('Ctrl Pts',(23.083555550122,40.9640157969843,38.366868585522)) ;
#15772 = CARTESIAN_POINT('Ctrl Pts',(22.9727407352119,39.2928539659985,37.8388953361349)) ;
#15773 = CARTESIAN_POINT('Ctrl Pts',(22.8619259203017,37.9396932227727,38.9526698287169)) ;
#15774 = CARTESIAN_POINT('Ctrl Pts',(22.7511111053916,38.136509477406,40.6941637216025)) ;
#15775 = CARTESIAN_POINT('Ctrl Pts',(22.6402962904815,39.7041127221009,41.4778458543625)) ;
#15776 = CARTESIAN_POINT('Ctrl Pts',(22.5294814755713,41.2152893427001,40.5902182080807)) ;
#15777 = CARTESIAN_POINT('Ctrl Pts',(22.4186666606612,41.2941989590302,38.8394152814942)) ;
#15778 = CARTESIAN_POINT('Ctrl Pts',(22.307851845751,39.8689988506925,37.8194435789608)) ;
#15779 = CARTESIAN_POINT('Ctrl Pts',(22.1970370308409,38.2372526771025,38.4589293400473)) ;
#15780 = CARTESIAN_POINT('Ctrl Pts',(22.0862222159307,37.884572533817,40.1756571344811)) ;
#15781 = CARTESIAN_POINT('Ctrl Pts',(21.9754074010206,39.1320536512838,41.4066439432543)) ;
#15782 = CARTESIAN_POINT('Ctrl Pts',(21.8645925861105,40.8439353794152,41.0311462414594)) ;
#15783 = CARTESIAN_POINT('Ctrl Pts',(21.7537777712003,41.4616468090319,39.3910334034537)) ;
#15784 = CARTESIAN_POINT('Ctrl Pts',(21.6429629562902,40.4227966905405,37.9795347660523)) ;
#15785 = CARTESIAN_POINT('Ctrl Pts',(21.53214814138,38.6731992203584,38.0817398511981)) ;
#15786 = CARTESIAN_POINT('Ctrl Pts',(21.4213333264699,37.8057629321309,39.6045961885133)) ;
#15787 = CARTESIAN_POINT('Ctrl Pts',(21.3105185115597,38.6102401857762,41.1616307819746)) ;
#15788 = CARTESIAN_POINT('Ctrl Pts',(21.1997036966497,40.3541982989288,41.3352499705511)) ;
#15789 = CARTESIAN_POINT('Ctrl Pts',(21.0888888817395,41.4498663517249,39.9673877570378)) ;
#15790 = CARTESIAN_POINT('Ctrl Pts',(20.9780740668294,40.8996933490919,38.3033961125266)) ;
#15791 = CARTESIAN_POINT('Ctrl Pts',(20.8672592519192,39.2045955811405,37.8582623699771)) ;
#15792 = CARTESIAN_POINT('Ctrl Pts',(20.7564444370091,37.907833098911,39.0372204078837)) ;
#15793 = CARTESIAN_POINT('Ctrl Pts',(20.6456296220989,38.1900944823029,40.7669660518425)) ;
#15794 = CARTESIAN_POINT('Ctrl Pts',(20.5348148071888,39.7942767797378,41.4725242667218)) ;
#15795 = CARTESIAN_POINT('Ctrl Pts',(20.4239999922786,41.260102964655,40.5118040569248)) ;
#15796 = CARTESIAN_POINT('Ctrl Pts',(20.3131851773685,41.2525427468677,38.758927890642)) ;
#15797 = CARTESIAN_POINT('Ctrl Pts',(20.2023703624584,39.7794361183673,37.8109065168399)) ;
#15798 = CARTESIAN_POINT('Ctrl Pts',(20.0915555475482,38.1800488939151,38.5286190989517)) ;
#15799 = CARTESIAN_POINT('Ctrl Pts',(19.9807407326381,37.9143916408252,40.2632216448386)) ;
#15800 = CARTESIAN_POINT('Ctrl Pts',(19.9068641893647,38.7822813061082,41.0372039405179)) ;
#15801 = CARTESIAN_POINT('Ctrl Pts',(19.8699259177279,39.2841766627494,41.1558877937552)) ;
#15802 = CARTESIAN_POINT('Origin',(29.4,39.642135623731,39.642135623731)) ;
#15803 = CARTESIAN_POINT('',(29.6,39.642135623731,41.796135623731)) ;
#15804 = CARTESIAN_POINT('Origin',(29.4,39.642135623731,41.796135623731)) ;
#15805 = CARTESIAN_POINT('Origin',(29.6,39.642135623731,39.642135623731)) ;
#15806 = CARTESIAN_POINT('Origin',(29.6,39.642135623731,39.642135623731)) ;
#15807 = CARTESIAN_POINT('Origin',(20.1,39.642135623731,39.642135623731)) ;
#15808 = CARTESIAN_POINT('Origin',(29.6,39.642135623731,39.642135623731)) ;
#15809 = CARTESIAN_POINT('',(29.6,39.642135623731,42.9421356237309)) ;
#15810 = CARTESIAN_POINT('Origin',(29.6,39.642135623731,39.642135623731)) ;
#15811 = CARTESIAN_POINT('Origin',(19.85,39.642135623731,39.642135623731)) ;
#15812 = CARTESIAN_POINT('',(19.6,39.642135623731,41.096135623731)) ;
#15813 = CARTESIAN_POINT('',(19.85,39.642135623731,41.346135623731)) ;
#15814 = CARTESIAN_POINT('Origin',(19.6,39.642135623731,39.642135623731)) ;
#15815 = CARTESIAN_POINT('Origin',(19.6,39.642135623731,39.642135623731)) ;
#15816 = CARTESIAN_POINT('Origin',(33.6,42.9412415963219,40.2238570189152)) ;
#15817 = CARTESIAN_POINT('',(33.35,42.9412415963219,40.2238570189152)) ;
#15818 = CARTESIAN_POINT('',(33.2,43.0755441166495,40.321625226856)) ;
#15819 = CARTESIAN_POINT('Ctrl Pts',(33.35,42.9412415963219,40.2238570189152)) ;
#15820 = CARTESIAN_POINT('Ctrl Pts',(33.2770142912005,43.0069223909349,40.2716706680543)) ;
#15821 = CARTESIAN_POINT('Ctrl Pts',(33.2,43.0755441166495,40.321625226856)) ;
#15822 = CARTESIAN_POINT('',(30.2,42.9412415963219,40.2238570189152)) ;
#15823 = CARTESIAN_POINT('',(33.6,42.9412415963219,40.2238570189152)) ;
#15824 = CARTESIAN_POINT('',(30.2,43.0755441166495,40.321625226856)) ;
#15825 = CARTESIAN_POINT('',(30.2,43.3462024860906,40.518656404528)) ;
#15826 = CARTESIAN_POINT('',(29.6,43.0755441166495,40.321625226856)) ;
#15827 = CARTESIAN_POINT('Origin',(30.2,43.1628233407496,40.2629278588902)) ;
#15828 = CARTESIAN_POINT('',(30.2,43.1008833801193,40.1779191226171)) ;
#15829 = CARTESIAN_POINT('Origin',(30.2,39.642135623731,39.642135623731)) ;
#15830 = CARTESIAN_POINT('',(30.2,42.9412415963219,40.2238570189152)) ;
#15831 = CARTESIAN_POINT('Origin',(33.6,43.4226076842641,40.0853409932026)) ;
#15832 = CARTESIAN_POINT('',(33.2,43.1008833801193,40.1779191226171)) ;
#15833 = CARTESIAN_POINT('Ctrl Pts',(33.2,43.1008833801193,40.1779191226171)) ;
#15834 = CARTESIAN_POINT('Ctrl Pts',(33.2770142911999,43.0193145854792,40.2013910404334)) ;
#15835 = CARTESIAN_POINT('Ctrl Pts',(33.35,42.9412415963219,40.2238570189152)) ;
#15836 = CARTESIAN_POINT('',(29.6,43.1008833801193,40.1779191226171)) ;
#15837 = CARTESIAN_POINT('Origin',(29.6,39.642135623731,39.642135623731)) ;
#15838 = CARTESIAN_POINT('',(33.2,43.1413750581413,39.7150971249983)) ;
#15839 = CARTESIAN_POINT('Origin',(33.2,39.642135623731,39.642135623731)) ;
#15840 = CARTESIAN_POINT('',(30.2,43.1413750581413,39.7150971249983)) ;
#15841 = CARTESIAN_POINT('',(29.6,43.1413750581413,39.7150971249983)) ;
#15842 = CARTESIAN_POINT('',(30.2,43.1413750581413,39.5691741224636)) ;
#15843 = CARTESIAN_POINT('Origin',(30.2,39.642135623731,39.642135623731)) ;
#15844 = CARTESIAN_POINT('',(33.2,43.1413750581413,39.5691741224636)) ;
#15845 = CARTESIAN_POINT('',(29.6,43.1413750581413,39.5691741224636)) ;
#15846 = CARTESIAN_POINT('',(33.2,43.1008833801193,39.1063521248448)) ;
#15847 = CARTESIAN_POINT('Origin',(33.2,39.642135623731,39.642135623731)) ;
#15848 = CARTESIAN_POINT('',(30.2,43.1008833801193,39.1063521248448)) ;
#15849 = CARTESIAN_POINT('',(29.6,43.1008833801193,39.1063521248448)) ;
#15850 = CARTESIAN_POINT('',(30.2,43.0755441166495,38.9626460206059)) ;
#15851 = CARTESIAN_POINT('Origin',(30.2,39.642135623731,39.642135623731)) ;
#15852 = CARTESIAN_POINT('',(33.2,43.0755441166495,38.9626460206059)) ;
#15853 = CARTESIAN_POINT('',(29.6,43.0755441166495,38.9626460206059)) ;
#15854 = CARTESIAN_POINT('',(33.2,42.9552994017302,38.5138866351854)) ;
#15855 = CARTESIAN_POINT('Origin',(33.2,39.642135623731,39.642135623731)) ;
#15856 = CARTESIAN_POINT('',(30.2,42.9552994017302,38.5138866351854)) ;
#15857 = CARTESIAN_POINT('',(29.6,42.9552994017302,38.5138866351854)) ;
#15858 = CARTESIAN_POINT('',(30.2,42.9053907954888,38.3767638665007)) ;
#15859 = CARTESIAN_POINT('Origin',(30.2,39.642135623731,39.642135623731)) ;
#15860 = CARTESIAN_POINT('',(33.2,42.9053907954888,38.3767638665007)) ;
#15861 = CARTESIAN_POINT('',(29.6,42.9053907954888,38.3767638665007)) ;
#15862 = CARTESIAN_POINT('',(33.2,42.7090466184883,37.9557024201215)) ;
#15863 = CARTESIAN_POINT('Origin',(33.2,39.642135623731,39.642135623731)) ;
#15864 = CARTESIAN_POINT('',(30.2,42.7090466184883,37.9557024201215)) ;
#15865 = CARTESIAN_POINT('',(29.6,42.7090466184883,37.9557024201215)) ;
#15866 = CARTESIAN_POINT('',(30.2,42.636085117221,37.82932939293)) ;
#15867 = CARTESIAN_POINT('Origin',(30.2,39.642135623731,39.642135623731)) ;
#15868 = CARTESIAN_POINT('',(33.2,42.636085117221,37.82932939293)) ;
#15869 = CARTESIAN_POINT('',(29.6,42.636085117221,37.82932939293)) ;
#15870 = CARTESIAN_POINT('',(33.2,42.3696072966026,37.4487596245729)) ;
#15871 = CARTESIAN_POINT('Origin',(33.2,39.642135623731,39.642135623731)) ;
#15872 = CARTESIAN_POINT('',(30.2,42.3696072966026,37.4487596245729)) ;
#15873 = CARTESIAN_POINT('',(29.6,42.3696072966026,37.4487596245729)) ;
#15874 = CARTESIAN_POINT('',(30.2,42.2758097986051,37.336976119358)) ;
#15875 = CARTESIAN_POINT('Origin',(30.2,39.642135623731,39.642135623731)) ;
#15876 = CARTESIAN_POINT('',(33.2,42.2758097986051,37.336976119358)) ;
#15877 = CARTESIAN_POINT('',(29.6,42.2758097986051,37.336976119358)) ;
#15878 = CARTESIAN_POINT('',(33.2,41.9472951281039,37.0084614488568)) ;
#15879 = CARTESIAN_POINT('Origin',(33.2,39.642135623731,39.642135623731)) ;
#15880 = CARTESIAN_POINT('',(30.2,41.9472951281039,37.0084614488568)) ;
#15881 = CARTESIAN_POINT('',(29.6,41.9472951281039,37.0084614488568)) ;
#15882 = CARTESIAN_POINT('',(30.2,41.835511622889,36.9146639508593)) ;
#15883 = CARTESIAN_POINT('Origin',(30.2,39.642135623731,39.642135623731)) ;
#15884 = CARTESIAN_POINT('',(33.2,41.835511622889,36.9146639508593)) ;
#15885 = CARTESIAN_POINT('',(29.6,41.835511622889,36.9146639508593)) ;
#15886 = CARTESIAN_POINT('',(33.2,41.4549418545319,36.6481861302409)) ;
#15887 = CARTESIAN_POINT('Origin',(33.2,39.642135623731,39.642135623731)) ;
#15888 = CARTESIAN_POINT('',(30.2,41.4549418545319,36.6481861302409)) ;
#15889 = CARTESIAN_POINT('',(29.6,41.4549418545319,36.6481861302409)) ;
#15890 = CARTESIAN_POINT('',(30.2,41.3285688273404,36.5752246289736)) ;
#15891 = CARTESIAN_POINT('Origin',(30.2,39.642135623731,39.642135623731)) ;
#15892 = CARTESIAN_POINT('',(33.2,41.3285688273404,36.5752246289736)) ;
#15893 = CARTESIAN_POINT('',(29.6,41.3285688273404,36.5752246289736)) ;
#15894 = CARTESIAN_POINT('',(33.2,40.9075073809612,36.3788804519731)) ;
#15895 = CARTESIAN_POINT('Origin',(33.2,39.642135623731,39.642135623731)) ;
#15896 = CARTESIAN_POINT('',(30.2,40.9075073809612,36.3788804519732)) ;
#15897 = CARTESIAN_POINT('',(29.6,40.9075073809612,36.3788804519731)) ;
#15898 = CARTESIAN_POINT('',(30.2,40.7703846122765,36.3289718457317)) ;
#15899 = CARTESIAN_POINT('Origin',(30.2,39.642135623731,39.642135623731)) ;
#15900 = CARTESIAN_POINT('',(33.2,40.7703846122765,36.3289718457317)) ;
#15901 = CARTESIAN_POINT('',(29.6,40.7703846122765,36.3289718457317)) ;
#15902 = CARTESIAN_POINT('',(33.2,40.321625226856,36.2087271308124)) ;
#15903 = CARTESIAN_POINT('Origin',(33.2,39.642135623731,39.642135623731)) ;
#15904 = CARTESIAN_POINT('',(30.2,40.321625226856,36.2087271308124)) ;
#15905 = CARTESIAN_POINT('',(29.6,40.321625226856,36.2087271308124)) ;
#15906 = CARTESIAN_POINT('',(30.2,40.1779191226171,36.1833878673426)) ;
#15907 = CARTESIAN_POINT('Origin',(30.2,39.642135623731,39.642135623731)) ;
#15908 = CARTESIAN_POINT('',(33.2,40.1779191226171,36.1833878673426)) ;
#15909 = CARTESIAN_POINT('',(29.6,40.1779191226171,36.1833878673426)) ;
#15910 = CARTESIAN_POINT('',(33.2,39.7150971249983,36.1428961893205)) ;
#15911 = CARTESIAN_POINT('Origin',(33.2,39.642135623731,39.642135623731)) ;
#15912 = CARTESIAN_POINT('',(30.2,39.7150971249983,36.1428961893206)) ;
#15913 = CARTESIAN_POINT('',(29.6,39.7150971249983,36.1428961893205)) ;
#15914 = CARTESIAN_POINT('',(30.2,39.5691741224637,36.1428961893205)) ;
#15915 = CARTESIAN_POINT('Origin',(30.2,39.642135623731,39.642135623731)) ;
#15916 = CARTESIAN_POINT('',(33.2,39.5691741224636,36.1428961893205)) ;
#15917 = CARTESIAN_POINT('',(29.6,39.5691741224636,36.1428961893205)) ;
#15918 = CARTESIAN_POINT('',(33.2,39.1063521248448,36.1833878673426)) ;
#15919 = CARTESIAN_POINT('Origin',(33.2,39.642135623731,39.642135623731)) ;
#15920 = CARTESIAN_POINT('',(30.2,39.1063521248448,36.1833878673426)) ;
#15921 = CARTESIAN_POINT('',(29.6,39.1063521248448,36.1833878673426)) ;
#15922 = CARTESIAN_POINT('',(30.2,38.9626460206059,36.2087271308124)) ;
#15923 = CARTESIAN_POINT('Origin',(30.2,39.642135623731,39.642135623731)) ;
#15924 = CARTESIAN_POINT('',(33.2,38.9626460206059,36.2087271308124)) ;
#15925 = CARTESIAN_POINT('',(29.6,38.9626460206059,36.2087271308124)) ;
#15926 = CARTESIAN_POINT('',(33.2,38.5138866351854,36.3289718457317)) ;
#15927 = CARTESIAN_POINT('Origin',(33.2,39.642135623731,39.642135623731)) ;
#15928 = CARTESIAN_POINT('',(30.2,38.5138866351854,36.3289718457317)) ;
#15929 = CARTESIAN_POINT('',(29.6,38.5138866351854,36.3289718457317)) ;
#15930 = CARTESIAN_POINT('',(30.2,38.3767638665007,36.3788804519731)) ;
#15931 = CARTESIAN_POINT('Origin',(30.2,39.642135623731,39.642135623731)) ;
#15932 = CARTESIAN_POINT('',(33.2,38.3767638665007,36.3788804519731)) ;
#15933 = CARTESIAN_POINT('',(29.6,38.3767638665007,36.3788804519731)) ;
#15934 = CARTESIAN_POINT('',(33.2,37.9557024201215,36.5752246289736)) ;
#15935 = CARTESIAN_POINT('Origin',(33.2,39.642135623731,39.642135623731)) ;
#15936 = CARTESIAN_POINT('',(30.2,37.9557024201215,36.5752246289736)) ;
#15937 = CARTESIAN_POINT('',(29.6,37.9557024201215,36.5752246289736)) ;
#15938 = CARTESIAN_POINT('',(30.2,37.82932939293,36.6481861302409)) ;
#15939 = CARTESIAN_POINT('Origin',(30.2,39.642135623731,39.642135623731)) ;
#15940 = CARTESIAN_POINT('',(33.2,37.82932939293,36.6481861302409)) ;
#15941 = CARTESIAN_POINT('',(29.6,37.82932939293,36.6481861302409)) ;
#15942 = CARTESIAN_POINT('',(33.2,37.4487596245729,36.9146639508593)) ;
#15943 = CARTESIAN_POINT('Origin',(33.2,39.642135623731,39.642135623731)) ;
#15944 = CARTESIAN_POINT('',(30.2,37.4487596245729,36.9146639508593)) ;
#15945 = CARTESIAN_POINT('',(29.6,37.4487596245729,36.9146639508593)) ;
#15946 = CARTESIAN_POINT('',(30.2,37.336976119358,37.0084614488568)) ;
#15947 = CARTESIAN_POINT('Origin',(30.2,39.642135623731,39.642135623731)) ;
#15948 = CARTESIAN_POINT('',(33.2,37.336976119358,37.0084614488568)) ;
#15949 = CARTESIAN_POINT('',(29.6,37.336976119358,37.0084614488568)) ;
#15950 = CARTESIAN_POINT('',(33.2,37.0084614488568,37.336976119358)) ;
#15951 = CARTESIAN_POINT('Origin',(33.2,39.642135623731,39.642135623731)) ;
#15952 = CARTESIAN_POINT('',(30.2,37.0084614488568,37.336976119358)) ;
#15953 = CARTESIAN_POINT('',(29.6,37.0084614488568,37.336976119358)) ;
#15954 = CARTESIAN_POINT('',(30.2,36.9146639508593,37.4487596245729)) ;
#15955 = CARTESIAN_POINT('Origin',(30.2,39.642135623731,39.642135623731)) ;
#15956 = CARTESIAN_POINT('',(33.2,36.9146639508593,37.4487596245729)) ;
#15957 = CARTESIAN_POINT('',(29.6,36.9146639508593,37.4487596245729)) ;
#15958 = CARTESIAN_POINT('',(33.2,36.6481861302409,37.82932939293)) ;
#15959 = CARTESIAN_POINT('Origin',(33.2,39.642135623731,39.642135623731)) ;
#15960 = CARTESIAN_POINT('',(30.2,36.6481861302409,37.82932939293)) ;
#15961 = CARTESIAN_POINT('',(29.6,36.6481861302409,37.82932939293)) ;
#15962 = CARTESIAN_POINT('',(30.2,36.5752246289736,37.9557024201215)) ;
#15963 = CARTESIAN_POINT('Origin',(30.2,39.642135623731,39.642135623731)) ;
#15964 = CARTESIAN_POINT('',(33.2,36.5752246289736,37.9557024201215)) ;
#15965 = CARTESIAN_POINT('',(29.6,36.5752246289736,37.9557024201215)) ;
#15966 = CARTESIAN_POINT('',(33.2,36.3788804519731,38.3767638665007)) ;
#15967 = CARTESIAN_POINT('Origin',(33.2,39.642135623731,39.642135623731)) ;
#15968 = CARTESIAN_POINT('',(30.2,36.3788804519731,38.3767638665007)) ;
#15969 = CARTESIAN_POINT('',(29.6,36.3788804519731,38.3767638665007)) ;
#15970 = CARTESIAN_POINT('',(30.2,36.3289718457317,38.5138866351854)) ;
#15971 = CARTESIAN_POINT('Origin',(30.2,39.642135623731,39.642135623731)) ;
#15972 = CARTESIAN_POINT('',(33.2,36.3289718457317,38.5138866351854)) ;
#15973 = CARTESIAN_POINT('',(29.6,36.3289718457317,38.5138866351854)) ;
#15974 = CARTESIAN_POINT('',(33.2,36.2087271308124,38.9626460206059)) ;
#15975 = CARTESIAN_POINT('Origin',(33.2,39.642135623731,39.642135623731)) ;
#15976 = CARTESIAN_POINT('',(30.2,36.2087271308124,38.9626460206059)) ;
#15977 = CARTESIAN_POINT('',(29.6,36.2087271308124,38.9626460206059)) ;
#15978 = CARTESIAN_POINT('',(30.2,36.1833878673426,39.1063521248448)) ;
#15979 = CARTESIAN_POINT('Origin',(30.2,39.642135623731,39.642135623731)) ;
#15980 = CARTESIAN_POINT('',(33.2,36.1833878673426,39.1063521248448)) ;
#15981 = CARTESIAN_POINT('',(29.6,36.1833878673426,39.1063521248448)) ;
#15982 = CARTESIAN_POINT('',(33.2,36.1428961893205,39.5691741224636)) ;
#15983 = CARTESIAN_POINT('Origin',(33.2,39.642135623731,39.642135623731)) ;
#15984 = CARTESIAN_POINT('',(30.2,36.1428961893205,39.5691741224636)) ;
#15985 = CARTESIAN_POINT('',(29.6,36.1428961893205,39.5691741224636)) ;
#15986 = CARTESIAN_POINT('',(30.2,36.1428961893206,39.7150971249983)) ;
#15987 = CARTESIAN_POINT('Origin',(30.2,39.642135623731,39.642135623731)) ;
#15988 = CARTESIAN_POINT('',(33.2,36.1428961893206,39.7150971249983)) ;
#15989 = CARTESIAN_POINT('',(29.6,36.1428961893206,39.7150971249983)) ;
#15990 = CARTESIAN_POINT('',(33.2,36.1833878673426,40.1779191226171)) ;
#15991 = CARTESIAN_POINT('Origin',(33.2,39.642135623731,39.642135623731)) ;
#15992 = CARTESIAN_POINT('',(30.2,36.1833878673426,40.1779191226171)) ;
#15993 = CARTESIAN_POINT('',(29.6,36.1833878673426,40.1779191226171)) ;
#15994 = CARTESIAN_POINT('',(30.2,36.2087271308124,40.321625226856)) ;
#15995 = CARTESIAN_POINT('Origin',(30.2,39.642135623731,39.642135623731)) ;
#15996 = CARTESIAN_POINT('',(33.2,36.2087271308124,40.321625226856)) ;
#15997 = CARTESIAN_POINT('',(29.6,36.2087271308124,40.321625226856)) ;
#15998 = CARTESIAN_POINT('',(33.2,36.3289718457317,40.7703846122765)) ;
#15999 = CARTESIAN_POINT('Origin',(33.2,39.642135623731,39.642135623731)) ;
#16000 = CARTESIAN_POINT('',(30.2,36.3289718457317,40.7703846122765)) ;
#16001 = CARTESIAN_POINT('',(29.6,36.3289718457317,40.7703846122765)) ;
#16002 = CARTESIAN_POINT('',(30.2,36.3788804519731,40.9075073809612)) ;
#16003 = CARTESIAN_POINT('Origin',(30.2,39.642135623731,39.642135623731)) ;
#16004 = CARTESIAN_POINT('',(33.2,36.3788804519731,40.9075073809612)) ;
#16005 = CARTESIAN_POINT('',(29.6,36.3788804519731,40.9075073809612)) ;
#16006 = CARTESIAN_POINT('',(33.2,36.5752246289736,41.3285688273404)) ;
#16007 = CARTESIAN_POINT('Origin',(33.2,39.642135623731,39.642135623731)) ;
#16008 = CARTESIAN_POINT('',(30.2,36.5752246289736,41.3285688273404)) ;
#16009 = CARTESIAN_POINT('',(29.6,36.5752246289736,41.3285688273404)) ;
#16010 = CARTESIAN_POINT('',(30.2,36.6481861302409,41.4549418545319)) ;
#16011 = CARTESIAN_POINT('Origin',(30.2,39.642135623731,39.642135623731)) ;
#16012 = CARTESIAN_POINT('',(33.2,36.6481861302409,41.4549418545319)) ;
#16013 = CARTESIAN_POINT('',(29.6,36.6481861302409,41.4549418545319)) ;
#16014 = CARTESIAN_POINT('',(33.2,36.9146639508593,41.835511622889)) ;
#16015 = CARTESIAN_POINT('Origin',(33.2,39.642135623731,39.642135623731)) ;
#16016 = CARTESIAN_POINT('',(30.2,36.9146639508593,41.835511622889)) ;
#16017 = CARTESIAN_POINT('',(29.6,36.9146639508593,41.835511622889)) ;
#16018 = CARTESIAN_POINT('',(30.2,37.0084614488568,41.9472951281039)) ;
#16019 = CARTESIAN_POINT('Origin',(30.2,39.642135623731,39.642135623731)) ;
#16020 = CARTESIAN_POINT('',(33.2,37.0084614488568,41.9472951281039)) ;
#16021 = CARTESIAN_POINT('',(29.6,37.0084614488568,41.9472951281039)) ;
#16022 = CARTESIAN_POINT('',(33.2,37.336976119358,42.2758097986051)) ;
#16023 = CARTESIAN_POINT('Origin',(33.2,39.642135623731,39.642135623731)) ;
#16024 = CARTESIAN_POINT('',(30.2,37.336976119358,42.2758097986051)) ;
#16025 = CARTESIAN_POINT('',(29.6,37.336976119358,42.2758097986051)) ;
#16026 = CARTESIAN_POINT('',(30.2,37.4487596245729,42.3696072966026)) ;
#16027 = CARTESIAN_POINT('Origin',(30.2,39.642135623731,39.642135623731)) ;
#16028 = CARTESIAN_POINT('',(33.2,37.4487596245729,42.3696072966026)) ;
#16029 = CARTESIAN_POINT('',(29.6,37.4487596245729,42.3696072966026)) ;
#16030 = CARTESIAN_POINT('',(33.2,37.82932939293,42.636085117221)) ;
#16031 = CARTESIAN_POINT('Origin',(33.2,39.642135623731,39.642135623731)) ;
#16032 = CARTESIAN_POINT('',(30.2,37.82932939293,42.636085117221)) ;
#16033 = CARTESIAN_POINT('',(29.6,37.82932939293,42.636085117221)) ;
#16034 = CARTESIAN_POINT('',(30.2,37.9557024201215,42.7090466184883)) ;
#16035 = CARTESIAN_POINT('Origin',(30.2,39.642135623731,39.642135623731)) ;
#16036 = CARTESIAN_POINT('',(33.2,37.9557024201215,42.7090466184883)) ;
#16037 = CARTESIAN_POINT('',(29.6,37.9557024201215,42.7090466184883)) ;
#16038 = CARTESIAN_POINT('',(33.2,38.3767638665007,42.9053907954887)) ;
#16039 = CARTESIAN_POINT('Origin',(33.2,39.642135623731,39.642135623731)) ;
#16040 = CARTESIAN_POINT('',(30.2,38.3767638665007,42.9053907954887)) ;
#16041 = CARTESIAN_POINT('',(29.6,38.3767638665007,42.9053907954887)) ;
#16042 = CARTESIAN_POINT('',(30.2,38.5138866351854,42.9552994017302)) ;
#16043 = CARTESIAN_POINT('Origin',(30.2,39.642135623731,39.642135623731)) ;
#16044 = CARTESIAN_POINT('',(33.2,38.5138866351854,42.9552994017302)) ;
#16045 = CARTESIAN_POINT('',(29.6,38.5138866351854,42.9552994017302)) ;
#16046 = CARTESIAN_POINT('',(33.2,38.9626460206059,43.0755441166495)) ;
#16047 = CARTESIAN_POINT('Origin',(33.2,39.642135623731,39.642135623731)) ;
#16048 = CARTESIAN_POINT('',(30.2,38.9626460206059,43.0755441166495)) ;
#16049 = CARTESIAN_POINT('',(29.6,38.9626460206059,43.0755441166495)) ;
#16050 = CARTESIAN_POINT('',(30.2,39.1063521248448,43.1008833801193)) ;
#16051 = CARTESIAN_POINT('Origin',(30.2,39.642135623731,39.642135623731)) ;
#16052 = CARTESIAN_POINT('',(33.2,39.1063521248448,43.1008833801193)) ;
#16053 = CARTESIAN_POINT('',(29.6,39.1063521248448,43.1008833801193)) ;
#16054 = CARTESIAN_POINT('',(33.2,39.5691741224636,43.1413750581413)) ;
#16055 = CARTESIAN_POINT('Origin',(33.2,39.642135623731,39.642135623731)) ;
#16056 = CARTESIAN_POINT('',(30.2,39.5691741224636,43.1413750581413)) ;
#16057 = CARTESIAN_POINT('',(29.6,39.5691741224636,43.1413750581413)) ;
#16058 = CARTESIAN_POINT('',(30.2,39.642135623731,43.142135623731)) ;
#16059 = CARTESIAN_POINT('Origin',(30.2,39.642135623731,39.642135623731)) ;
#16060 = CARTESIAN_POINT('',(29.8,39.642135623731,43.142135623731)) ;
#16061 = CARTESIAN_POINT('',(29.6,39.642135623731,43.142135623731)) ;
#16062 = CARTESIAN_POINT('Origin',(29.8,39.642135623731,39.642135623731)) ;
#16063 = CARTESIAN_POINT('',(30.2,39.7150971249983,43.1413750581413)) ;
#16064 = CARTESIAN_POINT('Origin',(30.2,39.642135623731,39.642135623731)) ;
#16065 = CARTESIAN_POINT('',(33.2,39.7150971249983,43.1413750581414)) ;
#16066 = CARTESIAN_POINT('',(29.6,39.7150971249983,43.1413750581414)) ;
#16067 = CARTESIAN_POINT('',(33.2,40.1779191226171,43.1008833801193)) ;
#16068 = CARTESIAN_POINT('Origin',(33.2,39.642135623731,39.642135623731)) ;
#16069 = CARTESIAN_POINT('',(30.2,40.1779191226171,43.1008833801193)) ;
#16070 = CARTESIAN_POINT('',(29.6,40.1779191226171,43.1008833801193)) ;
#16071 = CARTESIAN_POINT('',(30.2,40.321625226856,43.0755441166495)) ;
#16072 = CARTESIAN_POINT('Origin',(30.2,39.642135623731,39.642135623731)) ;
#16073 = CARTESIAN_POINT('',(33.2,40.321625226856,43.0755441166495)) ;
#16074 = CARTESIAN_POINT('',(29.6,40.321625226856,43.0755441166495)) ;
#16075 = CARTESIAN_POINT('',(33.2,40.7703846122765,42.9552994017302)) ;
#16076 = CARTESIAN_POINT('Origin',(33.2,39.642135623731,39.642135623731)) ;
#16077 = CARTESIAN_POINT('',(30.2,40.7703846122765,42.9552994017302)) ;
#16078 = CARTESIAN_POINT('',(29.6,40.7703846122765,42.9552994017302)) ;
#16079 = CARTESIAN_POINT('',(30.2,40.9075073809612,42.9053907954888)) ;
#16080 = CARTESIAN_POINT('Origin',(30.2,39.642135623731,39.642135623731)) ;
#16081 = CARTESIAN_POINT('',(33.2,40.9075073809612,42.9053907954888)) ;
#16082 = CARTESIAN_POINT('',(29.6,40.9075073809612,42.9053907954888)) ;
#16083 = CARTESIAN_POINT('',(33.2,41.3285688273404,42.7090466184883)) ;
#16084 = CARTESIAN_POINT('Origin',(33.2,39.642135623731,39.642135623731)) ;
#16085 = CARTESIAN_POINT('',(30.2,41.3285688273404,42.7090466184883)) ;
#16086 = CARTESIAN_POINT('',(29.6,41.3285688273404,42.7090466184883)) ;
#16087 = CARTESIAN_POINT('',(30.2,41.4549418545319,42.636085117221)) ;
#16088 = CARTESIAN_POINT('Origin',(30.2,39.642135623731,39.642135623731)) ;
#16089 = CARTESIAN_POINT('',(33.2,41.4549418545319,42.636085117221)) ;
#16090 = CARTESIAN_POINT('',(29.6,41.4549418545319,42.636085117221)) ;
#16091 = CARTESIAN_POINT('',(33.2,41.8355116228891,42.3696072966026)) ;
#16092 = CARTESIAN_POINT('Origin',(33.2,39.642135623731,39.642135623731)) ;
#16093 = CARTESIAN_POINT('',(30.2,41.835511622889,42.3696072966026)) ;
#16094 = CARTESIAN_POINT('',(29.6,41.8355116228891,42.3696072966026)) ;
#16095 = CARTESIAN_POINT('',(30.2,41.9472951281039,42.2758097986051)) ;
#16096 = CARTESIAN_POINT('Origin',(30.2,39.642135623731,39.642135623731)) ;
#16097 = CARTESIAN_POINT('',(33.2,41.9472951281039,42.2758097986051)) ;
#16098 = CARTESIAN_POINT('',(29.6,41.9472951281039,42.2758097986051)) ;
#16099 = CARTESIAN_POINT('',(33.2,42.2758097986051,41.9472951281039)) ;
#16100 = CARTESIAN_POINT('Origin',(33.2,39.642135623731,39.642135623731)) ;
#16101 = CARTESIAN_POINT('',(30.2,42.2758097986051,41.9472951281039)) ;
#16102 = CARTESIAN_POINT('',(29.6,42.2758097986051,41.9472951281039)) ;
#16103 = CARTESIAN_POINT('',(30.2,42.3696072966026,41.835511622889)) ;
#16104 = CARTESIAN_POINT('Origin',(30.2,39.642135623731,39.642135623731)) ;
#16105 = CARTESIAN_POINT('',(33.2,42.3696072966026,41.835511622889)) ;
#16106 = CARTESIAN_POINT('',(29.6,42.3696072966026,41.835511622889)) ;
#16107 = CARTESIAN_POINT('',(33.2,42.636085117221,41.4549418545319)) ;
#16108 = CARTESIAN_POINT('Origin',(33.2,39.642135623731,39.642135623731)) ;
#16109 = CARTESIAN_POINT('',(30.2,42.636085117221,41.4549418545319)) ;
#16110 = CARTESIAN_POINT('',(29.6,42.636085117221,41.4549418545319)) ;
#16111 = CARTESIAN_POINT('',(30.2,42.7090466184883,41.3285688273404)) ;
#16112 = CARTESIAN_POINT('Origin',(30.2,39.642135623731,39.642135623731)) ;
#16113 = CARTESIAN_POINT('',(33.2,42.7090466184883,41.3285688273404)) ;
#16114 = CARTESIAN_POINT('',(29.6,42.7090466184883,41.3285688273404)) ;
#16115 = CARTESIAN_POINT('',(33.2,42.9053907954888,40.9075073809612)) ;
#16116 = CARTESIAN_POINT('Origin',(33.2,39.642135623731,39.642135623731)) ;
#16117 = CARTESIAN_POINT('',(30.2,42.9053907954888,40.9075073809612)) ;
#16118 = CARTESIAN_POINT('',(29.6,42.9053907954888,40.9075073809612)) ;
#16119 = CARTESIAN_POINT('',(30.2,42.9552994017302,40.7703846122765)) ;
#16120 = CARTESIAN_POINT('Origin',(30.2,39.642135623731,39.642135623731)) ;
#16121 = CARTESIAN_POINT('',(33.2,42.9552994017302,40.7703846122765)) ;
#16122 = CARTESIAN_POINT('',(29.6,42.9552994017302,40.7703846122765)) ;
#16123 = CARTESIAN_POINT('Origin',(33.2,39.642135623731,39.642135623731)) ;
#16124 = CARTESIAN_POINT('Origin',(33.6,42.7901059033638,40.7879031038719)) ;
#16125 = CARTESIAN_POINT('',(33.35,42.7901059033638,40.7879031038719)) ;
#16126 = CARTESIAN_POINT('Ctrl Pts',(33.35,42.7901059033638,40.7879031038719)) ;
#16127 = CARTESIAN_POINT('Ctrl Pts',(33.2770142912003,42.8464861060822,40.8463957065364)) ;
#16128 = CARTESIAN_POINT('Ctrl Pts',(33.2,42.9053907954888,40.9075073809612)) ;
#16129 = CARTESIAN_POINT('',(30.2,42.7901059033638,40.7879031038719)) ;
#16130 = CARTESIAN_POINT('',(33.6,42.7901059033638,40.7879031038719)) ;
#16131 = CARTESIAN_POINT('',(30.2,43.1377231511858,41.1485445449414)) ;
#16132 = CARTESIAN_POINT('Origin',(30.2,43.0015367430406,40.8648576361202)) ;
#16133 = CARTESIAN_POINT('',(30.2,42.7901059033638,40.7879031038719)) ;
#16134 = CARTESIAN_POINT('Origin',(33.6,43.288212014249,40.7350797917956)) ;
#16135 = CARTESIAN_POINT('Ctrl Pts',(33.2,42.9552994017302,40.7703846122765)) ;
#16136 = CARTESIAN_POINT('Ctrl Pts',(33.2770142912003,42.8708939646091,40.7793356663763)) ;
#16137 = CARTESIAN_POINT('Ctrl Pts',(33.35,42.7901059033638,40.7879031038719)) ;
#16138 = CARTESIAN_POINT('Origin',(33.6,42.5433207264088,41.3171356237309)) ;
#16139 = CARTESIAN_POINT('',(33.35,42.5433207264088,41.3171356237309)) ;
#16140 = CARTESIAN_POINT('Ctrl Pts',(33.35,42.5433207264088,41.3171356237309)) ;
#16141 = CARTESIAN_POINT('Ctrl Pts',(33.2770142912008,42.5886872533023,41.3845299117868)) ;
#16142 = CARTESIAN_POINT('Ctrl Pts',(33.2,42.636085117221,41.4549418545319)) ;
#16143 = CARTESIAN_POINT('',(30.2,42.5433207264088,41.3171356237309)) ;
#16144 = CARTESIAN_POINT('',(33.6,42.5433207264088,41.3171356237309)) ;
#16145 = CARTESIAN_POINT('',(30.2,42.8230321581118,41.7326612125635)) ;
#16146 = CARTESIAN_POINT('Origin',(30.2,42.7381764422603,41.429635623731)) ;
#16147 = CARTESIAN_POINT('',(30.2,42.5433207264088,41.3171356237309)) ;
#16148 = CARTESIAN_POINT('Origin',(33.6,43.0430321581118,41.3516100348984)) ;
#16149 = CARTESIAN_POINT('Ctrl Pts',(33.2,42.7090466184883,41.3285688273404)) ;
#16150 = CARTESIAN_POINT('Ctrl Pts',(33.2770142912,42.6243691553829,41.3227270444743)) ;
#16151 = CARTESIAN_POINT('Ctrl Pts',(33.35,42.5433207264088,41.3171356237309)) ;
#16152 = CARTESIAN_POINT('Origin',(33.6,42.2083845081795,41.7954741161808)) ;
#16153 = CARTESIAN_POINT('',(33.35,42.2083845081795,41.7954741161808)) ;
#16154 = CARTESIAN_POINT('Ctrl Pts',(33.35,42.2083845081795,41.7954741161808)) ;
#16155 = CARTESIAN_POINT('Ctrl Pts',(33.2770142912003,42.2413589202856,41.8697223482896)) ;
#16156 = CARTESIAN_POINT('Ctrl Pts',(33.2,42.2758097986051,41.9472951281039)) ;
#16157 = CARTESIAN_POINT('',(30.2,42.2083845081795,41.7954741161808)) ;
#16158 = CARTESIAN_POINT('',(33.6,42.2083845081795,41.7954741161808)) ;
#16159 = CARTESIAN_POINT('',(30.2,42.411691233452,42.253258318026)) ;
#16160 = CARTESIAN_POINT('Origin',(30.2,42.3807445078813,41.9401013283603)) ;
#16161 = CARTESIAN_POINT('',(30.2,42.2083845081795,41.7954741161808)) ;
#16162 = CARTESIAN_POINT('Origin',(33.6,42.6945177817141,41.9161987630536)) ;
#16163 = CARTESIAN_POINT('Ctrl Pts',(33.2,42.3696072966026,41.8355116228891)) ;
#16164 = CARTESIAN_POINT('Ctrl Pts',(33.2770142912001,42.2872306893798,41.8150545026733)) ;
#16165 = CARTESIAN_POINT('Ctrl Pts',(33.35,42.2083845081795,41.7954741161808)) ;
#16166 = CARTESIAN_POINT('Origin',(33.6,41.7954741161809,42.2083845081795)) ;
#16167 = CARTESIAN_POINT('',(33.35,41.7954741161809,42.2083845081795)) ;
#16168 = CARTESIAN_POINT('Ctrl Pts',(33.35,41.7954741161809,42.2083845081795)) ;
#16169 = CARTESIAN_POINT('Ctrl Pts',(33.2770142912002,41.8150545026733,42.2872306893797)) ;
#16170 = CARTESIAN_POINT('Ctrl Pts',(33.2,41.8355116228891,42.3696072966026)) ;
#16171 = CARTESIAN_POINT('',(30.2,41.7954741161809,42.2083845081795)) ;
#16172 = CARTESIAN_POINT('',(33.6,41.7954741161809,42.2083845081795)) ;
#16173 = CARTESIAN_POINT('',(30.2,41.9161987630536,42.6945177817141)) ;
#16174 = CARTESIAN_POINT('Origin',(30.2,41.9401013283603,42.3807445078813)) ;
#16175 = CARTESIAN_POINT('',(30.2,41.7954741161809,42.2083845081795)) ;
#16176 = CARTESIAN_POINT('Origin',(33.6,42.253258318026,42.411691233452)) ;
#16177 = CARTESIAN_POINT('Ctrl Pts',(33.2,41.9472951281039,42.2758097986051)) ;
#16178 = CARTESIAN_POINT('Ctrl Pts',(33.2770142912005,41.8697223482895,42.2413589202856)) ;
#16179 = CARTESIAN_POINT('Ctrl Pts',(33.35,41.7954741161809,42.2083845081795)) ;
#16180 = CARTESIAN_POINT('Origin',(33.6,41.3171356237309,42.5433207264088)) ;
#16181 = CARTESIAN_POINT('',(33.35,41.3171356237309,42.5433207264088)) ;
#16182 = CARTESIAN_POINT('Ctrl Pts',(33.35,41.3171356237309,42.5433207264088)) ;
#16183 = CARTESIAN_POINT('Ctrl Pts',(33.2770142912002,41.3227270444743,42.6243691553827)) ;
#16184 = CARTESIAN_POINT('Ctrl Pts',(33.2,41.3285688273404,42.7090466184883)) ;
#16185 = CARTESIAN_POINT('',(30.2,41.3171356237309,42.5433207264088)) ;
#16186 = CARTESIAN_POINT('',(33.6,41.3171356237309,42.5433207264088)) ;
#16187 = CARTESIAN_POINT('',(30.2,41.3516100348984,43.0430321581118)) ;
#16188 = CARTESIAN_POINT('Origin',(30.2,41.429635623731,42.7381764422603)) ;
#16189 = CARTESIAN_POINT('',(30.2,41.3171356237309,42.5433207264088)) ;
#16190 = CARTESIAN_POINT('Origin',(33.6,41.7326612125635,42.8230321581118)) ;
#16191 = CARTESIAN_POINT('Ctrl Pts',(33.2,41.4549418545319,42.636085117221)) ;
#16192 = CARTESIAN_POINT('Ctrl Pts',(33.2770142912003,41.3845299117873,42.5886872533027)) ;
#16193 = CARTESIAN_POINT('Ctrl Pts',(33.35,41.3171356237309,42.5433207264088)) ;
#16194 = CARTESIAN_POINT('Origin',(33.6,40.7879031038719,42.7901059033638)) ;
#16195 = CARTESIAN_POINT('',(33.35,40.7879031038719,42.7901059033638)) ;
#16196 = CARTESIAN_POINT('Ctrl Pts',(33.35,40.7879031038719,42.7901059033638)) ;
#16197 = CARTESIAN_POINT('Ctrl Pts',(33.2770142912004,40.7793356663763,42.8708939646091)) ;
#16198 = CARTESIAN_POINT('Ctrl Pts',(33.2,40.7703846122765,42.9552994017302)) ;
#16199 = CARTESIAN_POINT('',(30.2,40.7879031038719,42.7901059033638)) ;
#16200 = CARTESIAN_POINT('',(33.6,40.7879031038719,42.7901059033638)) ;
#16201 = CARTESIAN_POINT('',(30.2,40.7350797917956,43.288212014249)) ;
#16202 = CARTESIAN_POINT('Origin',(30.2,40.8648576361202,43.0015367430406)) ;
#16203 = CARTESIAN_POINT('',(30.2,40.7879031038719,42.7901059033638)) ;
#16204 = CARTESIAN_POINT('Origin',(33.6,41.1485445449414,43.1377231511858)) ;
#16205 = CARTESIAN_POINT('Ctrl Pts',(33.2,40.9075073809612,42.9053907954888)) ;
#16206 = CARTESIAN_POINT('Ctrl Pts',(33.2770142912005,40.8463957065363,42.846486106082)) ;
#16207 = CARTESIAN_POINT('Ctrl Pts',(33.35,40.7879031038719,42.7901059033638)) ;
#16208 = CARTESIAN_POINT('Origin',(33.6,40.2238570189152,42.9412415963218)) ;
#16209 = CARTESIAN_POINT('',(33.35,40.2238570189152,42.9412415963218)) ;
#16210 = CARTESIAN_POINT('Ctrl Pts',(33.35,40.2238570189152,42.9412415963218)) ;
#16211 = CARTESIAN_POINT('Ctrl Pts',(33.2770142912001,40.2013910404334,43.019314585479)) ;
#16212 = CARTESIAN_POINT('Ctrl Pts',(33.2,40.1779191226171,43.1008833801193)) ;
#16213 = CARTESIAN_POINT('',(30.2,40.2238570189152,42.9412415963218)) ;
#16214 = CARTESIAN_POINT('',(33.6,40.2238570189152,42.9412415963218)) ;
#16215 = CARTESIAN_POINT('',(30.2,40.0853409932026,43.4226076842641)) ;
#16216 = CARTESIAN_POINT('Origin',(30.2,40.2629278588902,43.1628233407496)) ;
#16217 = CARTESIAN_POINT('',(30.2,40.2238570189152,42.9412415963218)) ;
#16218 = CARTESIAN_POINT('Origin',(33.6,40.518656404528,43.3462024860906)) ;
#16219 = CARTESIAN_POINT('Ctrl Pts',(33.2,40.321625226856,43.0755441166495)) ;
#16220 = CARTESIAN_POINT('Ctrl Pts',(33.2770142912007,40.2716706680542,43.0069223909347)) ;
#16221 = CARTESIAN_POINT('Ctrl Pts',(33.35,40.2238570189152,42.9412415963218)) ;
#16222 = CARTESIAN_POINT('Origin',(33.6,39.642135623731,42.992135623731)) ;
#16223 = CARTESIAN_POINT('',(33.35,39.642135623731,42.992135623731)) ;
#16224 = CARTESIAN_POINT('Ctrl Pts',(33.35,39.642135623731,42.992135623731)) ;
#16225 = CARTESIAN_POINT('Ctrl Pts',(33.2770142912005,39.6064537216512,43.0651213325304)) ;
#16226 = CARTESIAN_POINT('Ctrl Pts',(33.2,39.5691741224636,43.1413750581414)) ;
#16227 = CARTESIAN_POINT('',(30.2,39.642135623731,42.992135623731)) ;
#16228 = CARTESIAN_POINT('',(33.6,39.642135623731,42.992135623731)) ;
#16229 = CARTESIAN_POINT('',(30.2,39.422135623731,43.4421356237309)) ;
#16230 = CARTESIAN_POINT('Origin',(30.2,39.642135623731,43.2171356237309)) ;
#16231 = CARTESIAN_POINT('',(30.2,39.642135623731,42.992135623731)) ;
#16232 = CARTESIAN_POINT('Origin',(33.6,39.8621356237309,43.4421356237309)) ;
#16233 = CARTESIAN_POINT('Ctrl Pts',(33.2,39.7150971249983,43.1413750581414)) ;
#16234 = CARTESIAN_POINT('Ctrl Pts',(33.2770142912006,39.6778175258107,43.0651213325304)) ;
#16235 = CARTESIAN_POINT('Ctrl Pts',(33.35,39.642135623731,42.992135623731)) ;
#16236 = CARTESIAN_POINT('Origin',(33.6,39.0604142285467,42.9412415963219)) ;
#16237 = CARTESIAN_POINT('',(33.35,39.0604142285467,42.9412415963219)) ;
#16238 = CARTESIAN_POINT('Ctrl Pts',(33.35,39.0604142285467,42.9412415963219)) ;
#16239 = CARTESIAN_POINT('Ctrl Pts',(33.2770142912007,39.0126005794078,43.0069223909346)) ;
#16240 = CARTESIAN_POINT('Ctrl Pts',(33.2,38.9626460206059,43.0755441166495)) ;
#16241 = CARTESIAN_POINT('',(30.2,39.0604142285467,42.9412415963219)) ;
#16242 = CARTESIAN_POINT('',(33.6,39.0604142285467,42.9412415963219)) ;
#16243 = CARTESIAN_POINT('',(30.2,38.7656148429339,43.3462024860906)) ;
#16244 = CARTESIAN_POINT('Origin',(30.2,39.0213433885717,43.1628233407496)) ;
#16245 = CARTESIAN_POINT('',(30.2,39.0604142285467,42.9412415963219)) ;
#16246 = CARTESIAN_POINT('Origin',(33.6,39.1989302542593,43.4226076842641)) ;
#16247 = CARTESIAN_POINT('Ctrl Pts',(33.2,39.1063521248448,43.1008833801193)) ;
#16248 = CARTESIAN_POINT('Ctrl Pts',(33.2770142912004,39.0828802070284,43.0193145854787)) ;
#16249 = CARTESIAN_POINT('Ctrl Pts',(33.35,39.0604142285467,42.9412415963219)) ;
#16250 = CARTESIAN_POINT('Origin',(33.6,38.4963681435899,42.7901059033638)) ;
#16251 = CARTESIAN_POINT('',(33.35,38.4963681435899,42.7901059033638)) ;
#16252 = CARTESIAN_POINT('Ctrl Pts',(33.35,38.4963681435899,42.7901059033638)) ;
#16253 = CARTESIAN_POINT('Ctrl Pts',(33.2770142912005,38.4378755409257,42.846486106082)) ;
#16254 = CARTESIAN_POINT('Ctrl Pts',(33.2,38.3767638665007,42.9053907954888)) ;
#16255 = CARTESIAN_POINT('',(30.2,38.4963681435899,42.7901059033638)) ;
#16256 = CARTESIAN_POINT('',(33.6,38.4963681435899,42.7901059033638)) ;
#16257 = CARTESIAN_POINT('',(30.2,38.1357267025205,43.1377231511858)) ;
#16258 = CARTESIAN_POINT('Origin',(30.2,38.4194136113417,43.0015367430406)) ;
#16259 = CARTESIAN_POINT('',(30.2,38.4963681435899,42.7901059033638)) ;
#16260 = CARTESIAN_POINT('Origin',(33.6,38.5491914556663,43.288212014249)) ;
#16261 = CARTESIAN_POINT('Ctrl Pts',(33.2,38.5138866351854,42.9552994017302)) ;
#16262 = CARTESIAN_POINT('Ctrl Pts',(33.2770142912004,38.5049355810856,42.870893964609)) ;
#16263 = CARTESIAN_POINT('Ctrl Pts',(33.35,38.4963681435899,42.7901059033637)) ;
#16264 = CARTESIAN_POINT('Origin',(33.6,37.967135623731,42.5433207264088)) ;
#16265 = CARTESIAN_POINT('',(33.35,37.967135623731,42.5433207264088)) ;
#16266 = CARTESIAN_POINT('Ctrl Pts',(33.35,37.967135623731,42.5433207264088)) ;
#16267 = CARTESIAN_POINT('Ctrl Pts',(33.2770142912002,37.8997413356745,42.5886872533027)) ;
#16268 = CARTESIAN_POINT('Ctrl Pts',(33.2,37.82932939293,42.636085117221)) ;
#16269 = CARTESIAN_POINT('',(30.2,37.967135623731,42.5433207264088)) ;
#16270 = CARTESIAN_POINT('',(33.6,37.967135623731,42.5433207264088)) ;
#16271 = CARTESIAN_POINT('',(30.2,37.5516100348984,42.8230321581118)) ;
#16272 = CARTESIAN_POINT('Origin',(30.2,37.854635623731,42.7381764422603)) ;
#16273 = CARTESIAN_POINT('',(30.2,37.967135623731,42.5433207264088)) ;
#16274 = CARTESIAN_POINT('Origin',(33.6,37.9326612125635,43.0430321581118)) ;
#16275 = CARTESIAN_POINT('Ctrl Pts',(33.2,37.9557024201215,42.7090466184883)) ;
#16276 = CARTESIAN_POINT('Ctrl Pts',(33.2770142912003,37.9615442029876,42.6243691553826)) ;
#16277 = CARTESIAN_POINT('Ctrl Pts',(33.35,37.967135623731,42.5433207264088)) ;
#16278 = CARTESIAN_POINT('Origin',(33.6,37.488797131281,42.2083845081795)) ;
#16279 = CARTESIAN_POINT('',(33.35,37.488797131281,42.2083845081795)) ;
#16280 = CARTESIAN_POINT('Ctrl Pts',(33.35,37.488797131281,42.2083845081795)) ;
#16281 = CARTESIAN_POINT('Ctrl Pts',(33.2770142912006,37.4145488991726,42.2413589202855)) ;
#16282 = CARTESIAN_POINT('Ctrl Pts',(33.2,37.336976119358,42.2758097986051)) ;
#16283 = CARTESIAN_POINT('',(30.2,37.488797131281,42.2083845081795)) ;
#16284 = CARTESIAN_POINT('',(33.6,37.488797131281,42.2083845081795)) ;
#16285 = CARTESIAN_POINT('',(30.2,37.0310129294359,42.411691233452)) ;
#16286 = CARTESIAN_POINT('Origin',(30.2,37.3441699191016,42.3807445078813)) ;
#16287 = CARTESIAN_POINT('',(30.2,37.488797131281,42.2083845081795)) ;
#16288 = CARTESIAN_POINT('Origin',(33.6,37.3680724844083,42.6945177817141)) ;
#16289 = CARTESIAN_POINT('Ctrl Pts',(33.2,37.4487596245728,42.3696072966026)) ;
#16290 = CARTESIAN_POINT('Ctrl Pts',(33.2770142912007,37.4692167447887,42.2872306893791)) ;
#16291 = CARTESIAN_POINT('Ctrl Pts',(33.35,37.488797131281,42.2083845081795)) ;
#16292 = CARTESIAN_POINT('Origin',(33.6,37.0758867392824,41.7954741161808)) ;
#16293 = CARTESIAN_POINT('',(33.35,37.0758867392824,41.7954741161808)) ;
#16294 = CARTESIAN_POINT('Ctrl Pts',(33.35,37.0758867392824,41.7954741161808)) ;
#16295 = CARTESIAN_POINT('Ctrl Pts',(33.2770142912004,36.9970405580823,41.8150545026733)) ;
#16296 = CARTESIAN_POINT('Ctrl Pts',(33.2,36.9146639508593,41.835511622889)) ;
#16297 = CARTESIAN_POINT('',(30.2,37.0758867392824,41.7954741161808)) ;
#16298 = CARTESIAN_POINT('',(33.6,37.0758867392824,41.7954741161808)) ;
#16299 = CARTESIAN_POINT('',(30.2,36.5897534657478,41.9161987630536)) ;
#16300 = CARTESIAN_POINT('Origin',(30.2,36.9035267395806,41.9401013283603)) ;
#16301 = CARTESIAN_POINT('',(30.2,37.0758867392824,41.7954741161808)) ;
#16302 = CARTESIAN_POINT('Origin',(33.6,36.8725800140099,42.253258318026)) ;
#16303 = CARTESIAN_POINT('Ctrl Pts',(33.2,37.0084614488568,41.9472951281039)) ;
#16304 = CARTESIAN_POINT('Ctrl Pts',(33.2770142912006,37.0429123271764,41.8697223482894)) ;
#16305 = CARTESIAN_POINT('Ctrl Pts',(33.35,37.0758867392824,41.7954741161808)) ;
#16306 = CARTESIAN_POINT('Origin',(33.6,36.7409505210531,41.3171356237309)) ;
#16307 = CARTESIAN_POINT('',(33.35,36.7409505210531,41.3171356237309)) ;
#16308 = CARTESIAN_POINT('Ctrl Pts',(33.35,36.7409505210531,41.3171356237309)) ;
#16309 = CARTESIAN_POINT('Ctrl Pts',(33.2770142912004,36.6599020920795,41.3227270444743)) ;
#16310 = CARTESIAN_POINT('Ctrl Pts',(33.2,36.5752246289736,41.3285688273404)) ;
#16311 = CARTESIAN_POINT('',(30.2,36.7409505210531,41.3171356237309)) ;
#16312 = CARTESIAN_POINT('',(33.6,36.7409505210531,41.3171356237309)) ;
#16313 = CARTESIAN_POINT('',(30.2,36.2412390893501,41.3516100348984)) ;
#16314 = CARTESIAN_POINT('Origin',(30.2,36.5460948052016,41.4296356237309)) ;
#16315 = CARTESIAN_POINT('',(30.2,36.7409505210531,41.3171356237309)) ;
#16316 = CARTESIAN_POINT('Origin',(33.6,36.4612390893501,41.7326612125635)) ;
#16317 = CARTESIAN_POINT('Ctrl Pts',(33.2,36.6481861302409,41.4549418545319)) ;
#16318 = CARTESIAN_POINT('Ctrl Pts',(33.2770142912004,36.6955839941593,41.3845299117872)) ;
#16319 = CARTESIAN_POINT('Ctrl Pts',(33.35,36.7409505210531,41.3171356237309)) ;
#16320 = CARTESIAN_POINT('Origin',(33.6,36.4941653440982,40.7879031038719)) ;
#16321 = CARTESIAN_POINT('',(33.35,36.4941653440982,40.7879031038719)) ;
#16322 = CARTESIAN_POINT('Ctrl Pts',(33.35,36.4941653440982,40.7879031038719)) ;
#16323 = CARTESIAN_POINT('Ctrl Pts',(33.2770142912004,36.4133772828529,40.7793356663763)) ;
#16324 = CARTESIAN_POINT('Ctrl Pts',(33.2,36.3289718457317,40.7703846122765)) ;
#16325 = CARTESIAN_POINT('',(30.2,36.4941653440982,40.7879031038719)) ;
#16326 = CARTESIAN_POINT('',(33.6,36.4941653440982,40.7879031038719)) ;
#16327 = CARTESIAN_POINT('',(30.2,35.9960592332129,40.7350797917956)) ;
#16328 = CARTESIAN_POINT('Origin',(30.2,36.2827345044213,40.8648576361202)) ;
#16329 = CARTESIAN_POINT('',(30.2,36.4941653440982,40.7879031038719)) ;
#16330 = CARTESIAN_POINT('Origin',(33.6,36.1465480962761,41.1485445449414)) ;
#16331 = CARTESIAN_POINT('Ctrl Pts',(33.2,36.3788804519731,40.9075073809612)) ;
#16332 = CARTESIAN_POINT('Ctrl Pts',(33.2770142912005,36.4377851413799,40.8463957065362)) ;
#16333 = CARTESIAN_POINT('Ctrl Pts',(33.35,36.4941653440982,40.7879031038719)) ;
#16334 = CARTESIAN_POINT('Origin',(33.6,36.34302965114,40.2238570189152)) ;
#16335 = CARTESIAN_POINT('',(33.35,36.34302965114,40.2238570189152)) ;
#16336 = CARTESIAN_POINT('Ctrl Pts',(33.35,36.34302965114,40.2238570189152)) ;
#16337 = CARTESIAN_POINT('Ctrl Pts',(33.2770142912004,36.2649566619833,40.2013910404335)) ;
#16338 = CARTESIAN_POINT('Ctrl Pts',(33.2,36.1833878673426,40.1779191226171)) ;
#16339 = CARTESIAN_POINT('',(30.2,36.34302965114,40.2238570189152)) ;
#16340 = CARTESIAN_POINT('',(33.6,36.34302965114,40.2238570189152)) ;
#16341 = CARTESIAN_POINT('',(30.2,35.8616635631979,40.0853409932026)) ;
#16342 = CARTESIAN_POINT('Origin',(30.2,36.1214479067123,40.2629278588902)) ;
#16343 = CARTESIAN_POINT('',(30.2,36.34302965114,40.2238570189152)) ;
#16344 = CARTESIAN_POINT('Origin',(33.6,35.9380687613713,40.518656404528)) ;
#16345 = CARTESIAN_POINT('Ctrl Pts',(33.2,36.2087271308124,40.321625226856)) ;
#16346 = CARTESIAN_POINT('Ctrl Pts',(33.2770142912008,36.2773488565273,40.2716706680541)) ;
#16347 = CARTESIAN_POINT('Ctrl Pts',(33.35,36.34302965114,40.2238570189152)) ;
#16348 = CARTESIAN_POINT('Origin',(33.6,36.2921356237309,39.642135623731)) ;
#16349 = CARTESIAN_POINT('',(33.35,36.2921356237309,39.642135623731)) ;
#16350 = CARTESIAN_POINT('Ctrl Pts',(33.35,36.2921356237309,39.642135623731)) ;
#16351 = CARTESIAN_POINT('Ctrl Pts',(33.2770142912004,36.2191499149313,39.6064537216511)) ;
#16352 = CARTESIAN_POINT('Ctrl Pts',(33.2,36.1428961893205,39.5691741224637)) ;
#16353 = CARTESIAN_POINT('',(30.2,36.2921356237309,39.642135623731)) ;
#16354 = CARTESIAN_POINT('',(33.6,36.2921356237309,39.642135623731)) ;
#16355 = CARTESIAN_POINT('',(30.2,35.842135623731,39.422135623731)) ;
#16356 = CARTESIAN_POINT('Origin',(30.2,36.067135623731,39.642135623731)) ;
#16357 = CARTESIAN_POINT('',(30.2,36.2921356237309,39.642135623731)) ;
#16358 = CARTESIAN_POINT('Origin',(33.6,35.842135623731,39.862135623731)) ;
#16359 = CARTESIAN_POINT('Ctrl Pts',(33.2,36.1428961893205,39.7150971249983)) ;
#16360 = CARTESIAN_POINT('Ctrl Pts',(33.2770142912002,36.2191499149312,39.6778175258108)) ;
#16361 = CARTESIAN_POINT('Ctrl Pts',(33.35,36.2921356237309,39.642135623731)) ;
#16362 = CARTESIAN_POINT('Origin',(33.6,36.34302965114,39.0604142285467)) ;
#16363 = CARTESIAN_POINT('',(33.35,36.34302965114,39.0604142285467)) ;
#16364 = CARTESIAN_POINT('Ctrl Pts',(33.35,36.34302965114,39.0604142285467)) ;
#16365 = CARTESIAN_POINT('Ctrl Pts',(33.2770142912004,36.277348856527,39.0126005794075)) ;
#16366 = CARTESIAN_POINT('Ctrl Pts',(33.2,36.2087271308124,38.9626460206059)) ;
#16367 = CARTESIAN_POINT('',(30.2,36.34302965114,39.0604142285467)) ;
#16368 = CARTESIAN_POINT('',(33.6,36.34302965114,39.0604142285467)) ;
#16369 = CARTESIAN_POINT('',(30.2,35.9380687613713,38.7656148429339)) ;
#16370 = CARTESIAN_POINT('Origin',(30.2,36.1214479067123,39.0213433885717)) ;
#16371 = CARTESIAN_POINT('',(30.2,36.34302965114,39.0604142285467)) ;
#16372 = CARTESIAN_POINT('Origin',(33.6,35.8616635631978,39.1989302542593)) ;
#16373 = CARTESIAN_POINT('Ctrl Pts',(33.2,36.1833878673426,39.1063521248448)) ;
#16374 = CARTESIAN_POINT('Ctrl Pts',(33.2770142912004,36.2649566619833,39.0828802070284)) ;
#16375 = CARTESIAN_POINT('Ctrl Pts',(33.35,36.34302965114,39.0604142285467)) ;
#16376 = CARTESIAN_POINT('Origin',(33.6,36.4941653440982,38.49636814359)) ;
#16377 = CARTESIAN_POINT('',(33.35,36.4941653440982,38.49636814359)) ;
#16378 = CARTESIAN_POINT('Ctrl Pts',(33.35,36.4941653440982,38.49636814359)) ;
#16379 = CARTESIAN_POINT('Ctrl Pts',(33.2770142912005,36.4377851413798,38.4378755409256)) ;
#16380 = CARTESIAN_POINT('Ctrl Pts',(33.2,36.3788804519731,38.3767638665007)) ;
#16381 = CARTESIAN_POINT('',(30.2,36.4941653440982,38.49636814359)) ;
#16382 = CARTESIAN_POINT('',(33.6,36.4941653440982,38.49636814359)) ;
#16383 = CARTESIAN_POINT('',(30.2,36.1465480962762,38.1357267025205)) ;
#16384 = CARTESIAN_POINT('Origin',(30.2,36.2827345044213,38.4194136113417)) ;
#16385 = CARTESIAN_POINT('',(30.2,36.4941653440982,38.49636814359)) ;
#16386 = CARTESIAN_POINT('Origin',(33.6,35.9960592332129,38.5491914556663)) ;
#16387 = CARTESIAN_POINT('Ctrl Pts',(33.2,36.3289718457317,38.5138866351854)) ;
#16388 = CARTESIAN_POINT('Ctrl Pts',(33.2770142912004,36.4133772828529,38.5049355810856)) ;
#16389 = CARTESIAN_POINT('Ctrl Pts',(33.35,36.4941653440982,38.49636814359)) ;
#16390 = CARTESIAN_POINT('Origin',(33.6,36.7409505210531,37.9671356237309)) ;
#16391 = CARTESIAN_POINT('',(33.35,36.7409505210531,37.9671356237309)) ;
#16392 = CARTESIAN_POINT('Ctrl Pts',(33.35,36.7409505210531,37.9671356237309)) ;
#16393 = CARTESIAN_POINT('Ctrl Pts',(33.2770142912005,36.6955839941594,37.8997413356748)) ;
#16394 = CARTESIAN_POINT('Ctrl Pts',(33.2,36.6481861302409,37.82932939293)) ;
#16395 = CARTESIAN_POINT('',(30.2,36.7409505210531,37.9671356237309)) ;
#16396 = CARTESIAN_POINT('',(33.6,36.7409505210531,37.9671356237309)) ;
#16397 = CARTESIAN_POINT('',(30.2,36.4612390893501,37.5516100348984)) ;
#16398 = CARTESIAN_POINT('Origin',(30.2,36.5460948052016,37.8546356237309)) ;
#16399 = CARTESIAN_POINT('',(30.2,36.7409505210531,37.9671356237309)) ;
#16400 = CARTESIAN_POINT('Origin',(33.6,36.2412390893501,37.9326612125635)) ;
#16401 = CARTESIAN_POINT('Ctrl Pts',(33.2,36.5752246289736,37.9557024201215)) ;
#16402 = CARTESIAN_POINT('Ctrl Pts',(33.2770142912003,36.6599020920794,37.9615442029876)) ;
#16403 = CARTESIAN_POINT('Ctrl Pts',(33.35,36.7409505210531,37.9671356237309)) ;
#16404 = CARTESIAN_POINT('Origin',(33.6,37.0758867392824,37.488797131281)) ;
#16405 = CARTESIAN_POINT('',(33.35,37.0758867392824,37.488797131281)) ;
#16406 = CARTESIAN_POINT('Ctrl Pts',(33.35,37.0758867392824,37.488797131281)) ;
#16407 = CARTESIAN_POINT('Ctrl Pts',(33.2770142912006,37.0429123271764,37.4145488991725)) ;
#16408 = CARTESIAN_POINT('Ctrl Pts',(33.2,37.0084614488568,37.336976119358)) ;
#16409 = CARTESIAN_POINT('',(30.2,37.0758867392824,37.488797131281)) ;
#16410 = CARTESIAN_POINT('',(33.6,37.0758867392824,37.488797131281)) ;
#16411 = CARTESIAN_POINT('',(30.2,36.8725800140099,37.0310129294359)) ;
#16412 = CARTESIAN_POINT('Origin',(30.2,36.9035267395806,37.3441699191016)) ;
#16413 = CARTESIAN_POINT('',(30.2,37.0758867392824,37.488797131281)) ;
#16414 = CARTESIAN_POINT('Origin',(33.6,36.5897534657478,37.3680724844083)) ;
#16415 = CARTESIAN_POINT('Ctrl Pts',(33.2,36.9146639508593,37.4487596245728)) ;
#16416 = CARTESIAN_POINT('Ctrl Pts',(33.2770142912007,36.9970405580828,37.4692167447887)) ;
#16417 = CARTESIAN_POINT('Ctrl Pts',(33.35,37.0758867392824,37.488797131281)) ;
#16418 = CARTESIAN_POINT('Origin',(33.6,37.488797131281,37.0758867392824)) ;
#16419 = CARTESIAN_POINT('',(33.35,37.488797131281,37.0758867392824)) ;
#16420 = CARTESIAN_POINT('Ctrl Pts',(33.35,37.488797131281,37.0758867392824)) ;
#16421 = CARTESIAN_POINT('Ctrl Pts',(33.2770142912005,37.4692167447886,36.9970405580825)) ;
#16422 = CARTESIAN_POINT('Ctrl Pts',(33.2,37.4487596245729,36.9146639508593)) ;
#16423 = CARTESIAN_POINT('',(30.2,37.488797131281,37.0758867392824)) ;
#16424 = CARTESIAN_POINT('',(33.6,37.488797131281,37.0758867392824)) ;
#16425 = CARTESIAN_POINT('',(30.2,37.3680724844083,36.5897534657478)) ;
#16426 = CARTESIAN_POINT('Origin',(30.2,37.3441699191016,36.9035267395806)) ;
#16427 = CARTESIAN_POINT('',(30.2,37.488797131281,37.0758867392824)) ;
#16428 = CARTESIAN_POINT('Origin',(33.6,37.0310129294359,36.8725800140099)) ;
#16429 = CARTESIAN_POINT('Ctrl Pts',(33.2,37.336976119358,37.0084614488568)) ;
#16430 = CARTESIAN_POINT('Ctrl Pts',(33.2770142912005,37.4145488991724,37.0429123271763)) ;
#16431 = CARTESIAN_POINT('Ctrl Pts',(33.35,37.488797131281,37.0758867392824)) ;
#16432 = CARTESIAN_POINT('Origin',(33.6,37.967135623731,36.7409505210531)) ;
#16433 = CARTESIAN_POINT('',(33.35,37.967135623731,36.7409505210531)) ;
#16434 = CARTESIAN_POINT('Ctrl Pts',(33.35,37.967135623731,36.7409505210531)) ;
#16435 = CARTESIAN_POINT('Ctrl Pts',(33.2770142912002,37.9615442029876,36.6599020920793)) ;
#16436 = CARTESIAN_POINT('Ctrl Pts',(33.2,37.9557024201215,36.5752246289736)) ;
#16437 = CARTESIAN_POINT('',(30.2,37.967135623731,36.7409505210531)) ;
#16438 = CARTESIAN_POINT('',(33.6,37.967135623731,36.7409505210531)) ;
#16439 = CARTESIAN_POINT('',(30.2,37.9326612125635,36.2412390893501)) ;
#16440 = CARTESIAN_POINT('Origin',(30.2,37.854635623731,36.5460948052016)) ;
#16441 = CARTESIAN_POINT('',(30.2,37.967135623731,36.7409505210531)) ;
#16442 = CARTESIAN_POINT('Origin',(33.6,37.5516100348984,36.4612390893501)) ;
#16443 = CARTESIAN_POINT('Ctrl Pts',(33.2,37.82932939293,36.6481861302409)) ;
#16444 = CARTESIAN_POINT('Ctrl Pts',(33.2770142912006,37.8997413356749,36.6955839941594)) ;
#16445 = CARTESIAN_POINT('Ctrl Pts',(33.35,37.967135623731,36.7409505210531)) ;
#16446 = CARTESIAN_POINT('Origin',(33.6,38.49636814359,36.4941653440981)) ;
#16447 = CARTESIAN_POINT('',(33.35,38.49636814359,36.4941653440981)) ;
#16448 = CARTESIAN_POINT('Ctrl Pts',(33.35,38.49636814359,36.4941653440981)) ;
#16449 = CARTESIAN_POINT('Ctrl Pts',(33.2770142912006,38.5049355810856,36.4133772828531)) ;
#16450 = CARTESIAN_POINT('Ctrl Pts',(33.2,38.5138866351854,36.3289718457317)) ;
#16451 = CARTESIAN_POINT('',(30.2,38.49636814359,36.4941653440981)) ;
#16452 = CARTESIAN_POINT('',(33.6,38.49636814359,36.4941653440981)) ;
#16453 = CARTESIAN_POINT('',(30.2,38.5491914556663,35.9960592332129)) ;
#16454 = CARTESIAN_POINT('Origin',(30.2,38.4194136113417,36.2827345044213)) ;
#16455 = CARTESIAN_POINT('',(30.2,38.49636814359,36.4941653440981)) ;
#16456 = CARTESIAN_POINT('Origin',(33.6,38.1357267025205,36.1465480962761)) ;
#16457 = CARTESIAN_POINT('Ctrl Pts',(33.2,38.3767638665007,36.3788804519731)) ;
#16458 = CARTESIAN_POINT('Ctrl Pts',(33.2770142912005,38.4378755409256,36.4377851413798)) ;
#16459 = CARTESIAN_POINT('Ctrl Pts',(33.35,38.49636814359,36.4941653440981)) ;
#16460 = CARTESIAN_POINT('Origin',(33.6,39.0604142285467,36.34302965114)) ;
#16461 = CARTESIAN_POINT('',(33.35,39.0604142285467,36.34302965114)) ;
#16462 = CARTESIAN_POINT('Ctrl Pts',(33.35,39.0604142285467,36.34302965114)) ;
#16463 = CARTESIAN_POINT('Ctrl Pts',(33.2770142912002,39.0828802070284,36.2649566619831)) ;
#16464 = CARTESIAN_POINT('Ctrl Pts',(33.2,39.1063521248448,36.1833878673426)) ;
#16465 = CARTESIAN_POINT('',(30.2,39.0604142285467,36.34302965114)) ;
#16466 = CARTESIAN_POINT('',(33.6,39.0604142285467,36.34302965114)) ;
#16467 = CARTESIAN_POINT('',(30.2,39.1989302542593,35.8616635631978)) ;
#16468 = CARTESIAN_POINT('Origin',(30.2,39.0213433885717,36.1214479067123)) ;
#16469 = CARTESIAN_POINT('',(30.2,39.0604142285467,36.34302965114)) ;
#16470 = CARTESIAN_POINT('Origin',(33.6,38.7656148429339,35.9380687613713)) ;
#16471 = CARTESIAN_POINT('Ctrl Pts',(33.2,38.9626460206059,36.2087271308124)) ;
#16472 = CARTESIAN_POINT('Ctrl Pts',(33.2770142912006,39.0126005794077,36.2773488565272)) ;
#16473 = CARTESIAN_POINT('Ctrl Pts',(33.35,39.0604142285467,36.34302965114)) ;
#16474 = CARTESIAN_POINT('Origin',(33.6,39.642135623731,36.2921356237309)) ;
#16475 = CARTESIAN_POINT('',(33.35,39.642135623731,36.2921356237309)) ;
#16476 = CARTESIAN_POINT('Ctrl Pts',(33.35,39.642135623731,36.2921356237309)) ;
#16477 = CARTESIAN_POINT('Ctrl Pts',(33.2770142912005,39.6778175258107,36.2191499149314)) ;
#16478 = CARTESIAN_POINT('Ctrl Pts',(33.2,39.7150971249983,36.1428961893205)) ;
#16479 = CARTESIAN_POINT('',(30.2,39.642135623731,36.2921356237309)) ;
#16480 = CARTESIAN_POINT('',(33.6,39.642135623731,36.2921356237309)) ;
#16481 = CARTESIAN_POINT('',(30.2,39.8621356237309,35.8421356237309)) ;
#16482 = CARTESIAN_POINT('Origin',(30.2,39.642135623731,36.0671356237309)) ;
#16483 = CARTESIAN_POINT('',(30.2,39.642135623731,36.2921356237309)) ;
#16484 = CARTESIAN_POINT('Origin',(33.6,39.422135623731,35.8421356237309)) ;
#16485 = CARTESIAN_POINT('Ctrl Pts',(33.2,39.5691741224637,36.1428961893205)) ;
#16486 = CARTESIAN_POINT('Ctrl Pts',(33.2770142912005,39.6064537216512,36.2191499149315)) ;
#16487 = CARTESIAN_POINT('Ctrl Pts',(33.35,39.642135623731,36.2921356237309)) ;
#16488 = CARTESIAN_POINT('Origin',(33.6,40.2238570189152,36.34302965114)) ;
#16489 = CARTESIAN_POINT('',(33.35,40.2238570189152,36.34302965114)) ;
#16490 = CARTESIAN_POINT('Ctrl Pts',(33.35,40.2238570189152,36.34302965114)) ;
#16491 = CARTESIAN_POINT('Ctrl Pts',(33.2770142912005,40.2716706680543,36.277348856527)) ;
#16492 = CARTESIAN_POINT('Ctrl Pts',(33.2,40.321625226856,36.2087271308124)) ;
#16493 = CARTESIAN_POINT('',(30.2,40.2238570189152,36.34302965114)) ;
#16494 = CARTESIAN_POINT('',(33.6,40.2238570189152,36.34302965114)) ;
#16495 = CARTESIAN_POINT('',(30.2,40.518656404528,35.9380687613713)) ;
#16496 = CARTESIAN_POINT('Origin',(30.2,40.2629278588902,36.1214479067123)) ;
#16497 = CARTESIAN_POINT('',(30.2,40.2238570189152,36.34302965114)) ;
#16498 = CARTESIAN_POINT('Origin',(33.6,40.0853409932026,35.8616635631978)) ;
#16499 = CARTESIAN_POINT('Ctrl Pts',(33.2,40.1779191226171,36.1833878673426)) ;
#16500 = CARTESIAN_POINT('Ctrl Pts',(33.2770142912004,40.2013910404335,36.2649566619833)) ;
#16501 = CARTESIAN_POINT('Ctrl Pts',(33.35,40.2238570189152,36.34302965114)) ;
#16502 = CARTESIAN_POINT('Origin',(33.6,40.7879031038719,36.4941653440982)) ;
#16503 = CARTESIAN_POINT('',(33.35,40.7879031038719,36.4941653440982)) ;
#16504 = CARTESIAN_POINT('Ctrl Pts',(33.35,40.7879031038719,36.4941653440982)) ;
#16505 = CARTESIAN_POINT('Ctrl Pts',(33.2770142912003,40.8463957065363,36.4377851413798)) ;
#16506 = CARTESIAN_POINT('Ctrl Pts',(33.2,40.9075073809612,36.3788804519731)) ;
#16507 = CARTESIAN_POINT('',(30.2,40.7879031038719,36.4941653440982)) ;
#16508 = CARTESIAN_POINT('',(33.6,40.7879031038719,36.4941653440982)) ;
#16509 = CARTESIAN_POINT('',(30.2,41.1485445449414,36.1465480962762)) ;
#16510 = CARTESIAN_POINT('Origin',(30.2,40.8648576361202,36.2827345044213)) ;
#16511 = CARTESIAN_POINT('',(30.2,40.7879031038719,36.4941653440982)) ;
#16512 = CARTESIAN_POINT('Origin',(33.6,40.7350797917956,35.9960592332129)) ;
#16513 = CARTESIAN_POINT('Ctrl Pts',(33.2,40.7703846122765,36.3289718457317)) ;
#16514 = CARTESIAN_POINT('Ctrl Pts',(33.2770142912004,40.7793356663763,36.4133772828528)) ;
#16515 = CARTESIAN_POINT('Ctrl Pts',(33.35,40.7879031038719,36.4941653440982)) ;
#16516 = CARTESIAN_POINT('Origin',(33.6,41.3171356237309,36.7409505210531)) ;
#16517 = CARTESIAN_POINT('',(33.35,41.3171356237309,36.7409505210531)) ;
#16518 = CARTESIAN_POINT('Ctrl Pts',(33.35,41.3171356237309,36.7409505210531)) ;
#16519 = CARTESIAN_POINT('Ctrl Pts',(33.277014291201,41.3845299117866,36.6955839941597)) ;
#16520 = CARTESIAN_POINT('Ctrl Pts',(33.2,41.4549418545319,36.6481861302409)) ;
#16521 = CARTESIAN_POINT('',(30.2,41.3171356237309,36.7409505210531)) ;
#16522 = CARTESIAN_POINT('',(33.6,41.3171356237309,36.7409505210531)) ;
#16523 = CARTESIAN_POINT('',(30.2,41.7326612125635,36.4612390893501)) ;
#16524 = CARTESIAN_POINT('Origin',(30.2,41.429635623731,36.5460948052016)) ;
#16525 = CARTESIAN_POINT('',(30.2,41.3171356237309,36.7409505210531)) ;
#16526 = CARTESIAN_POINT('Origin',(33.6,41.3516100348984,36.2412390893501)) ;
#16527 = CARTESIAN_POINT('Ctrl Pts',(33.2,41.3285688273404,36.5752246289736)) ;
#16528 = CARTESIAN_POINT('Ctrl Pts',(33.2770142912007,41.3227270444743,36.6599020920798)) ;
#16529 = CARTESIAN_POINT('Ctrl Pts',(33.35,41.3171356237309,36.7409505210531)) ;
#16530 = CARTESIAN_POINT('Origin',(33.6,41.7954741161808,37.0758867392824)) ;
#16531 = CARTESIAN_POINT('',(33.35,41.7954741161808,37.0758867392824)) ;
#16532 = CARTESIAN_POINT('Ctrl Pts',(33.35,41.7954741161808,37.0758867392824)) ;
#16533 = CARTESIAN_POINT('Ctrl Pts',(33.2770142912011,41.8697223482889,37.0429123271766)) ;
#16534 = CARTESIAN_POINT('Ctrl Pts',(33.2,41.9472951281039,37.0084614488568)) ;
#16535 = CARTESIAN_POINT('',(30.2,41.7954741161808,37.0758867392824)) ;
#16536 = CARTESIAN_POINT('',(33.6,41.7954741161808,37.0758867392824)) ;
#16537 = CARTESIAN_POINT('',(30.2,42.253258318026,36.8725800140099)) ;
#16538 = CARTESIAN_POINT('Origin',(30.2,41.9401013283603,36.9035267395806)) ;
#16539 = CARTESIAN_POINT('',(30.2,41.7954741161808,37.0758867392824)) ;
#16540 = CARTESIAN_POINT('Origin',(33.6,41.9161987630536,36.5897534657478)) ;
#16541 = CARTESIAN_POINT('Ctrl Pts',(33.2,41.835511622889,36.9146639508593)) ;
#16542 = CARTESIAN_POINT('Ctrl Pts',(33.2770142912009,41.8150545026731,36.9970405580829)) ;
#16543 = CARTESIAN_POINT('Ctrl Pts',(33.35,41.7954741161808,37.0758867392824)) ;
#16544 = CARTESIAN_POINT('Origin',(33.6,42.2083845081795,37.488797131281)) ;
#16545 = CARTESIAN_POINT('',(33.35,42.2083845081795,37.488797131281)) ;
#16546 = CARTESIAN_POINT('Ctrl Pts',(33.35,42.2083845081795,37.488797131281)) ;
#16547 = CARTESIAN_POINT('Ctrl Pts',(33.2770142912011,42.2872306893787,37.4692167447888)) ;
#16548 = CARTESIAN_POINT('Ctrl Pts',(33.2,42.3696072966026,37.4487596245728)) ;
#16549 = CARTESIAN_POINT('',(30.2,42.2083845081795,37.488797131281)) ;
#16550 = CARTESIAN_POINT('',(33.6,42.2083845081795,37.488797131281)) ;
#16551 = CARTESIAN_POINT('',(30.2,42.6945177817141,37.3680724844083)) ;
#16552 = CARTESIAN_POINT('Origin',(30.2,42.3807445078813,37.3441699191016)) ;
#16553 = CARTESIAN_POINT('',(30.2,42.2083845081795,37.488797131281)) ;
#16554 = CARTESIAN_POINT('Origin',(33.6,42.411691233452,37.0310129294359)) ;
#16555 = CARTESIAN_POINT('Ctrl Pts',(33.2,42.2758097986051,37.336976119358)) ;
#16556 = CARTESIAN_POINT('Ctrl Pts',(33.2770142912009,42.2413589202854,37.4145488991728)) ;
#16557 = CARTESIAN_POINT('Ctrl Pts',(33.35,42.2083845081795,37.488797131281)) ;
#16558 = CARTESIAN_POINT('Origin',(33.6,42.5433207264088,37.967135623731)) ;
#16559 = CARTESIAN_POINT('',(33.35,42.5433207264088,37.967135623731)) ;
#16560 = CARTESIAN_POINT('Ctrl Pts',(33.35,42.5433207264088,37.967135623731)) ;
#16561 = CARTESIAN_POINT('Ctrl Pts',(33.2770142912005,42.6243691553823,37.9615442029876)) ;
#16562 = CARTESIAN_POINT('Ctrl Pts',(33.2,42.7090466184883,37.9557024201215)) ;
#16563 = CARTESIAN_POINT('',(30.2,42.5433207264088,37.967135623731)) ;
#16564 = CARTESIAN_POINT('',(33.6,42.5433207264088,37.967135623731)) ;
#16565 = CARTESIAN_POINT('',(30.2,43.0430321581118,37.9326612125635)) ;
#16566 = CARTESIAN_POINT('Origin',(30.2,42.7381764422603,37.854635623731)) ;
#16567 = CARTESIAN_POINT('',(30.2,42.5433207264088,37.967135623731)) ;
#16568 = CARTESIAN_POINT('Origin',(33.6,42.8230321581118,37.5516100348984)) ;
#16569 = CARTESIAN_POINT('Ctrl Pts',(33.2,42.636085117221,37.82932939293)) ;
#16570 = CARTESIAN_POINT('Ctrl Pts',(33.2770142912006,42.5886872533024,37.8997413356749)) ;
#16571 = CARTESIAN_POINT('Ctrl Pts',(33.35,42.5433207264088,37.967135623731)) ;
#16572 = CARTESIAN_POINT('Origin',(33.6,42.7901059033638,38.49636814359)) ;
#16573 = CARTESIAN_POINT('',(33.35,42.7901059033638,38.49636814359)) ;
#16574 = CARTESIAN_POINT('Ctrl Pts',(33.35,42.7901059033638,38.49636814359)) ;
#16575 = CARTESIAN_POINT('Ctrl Pts',(33.2770142912007,42.8708939646087,38.5049355810856)) ;
#16576 = CARTESIAN_POINT('Ctrl Pts',(33.2,42.9552994017302,38.5138866351854)) ;
#16577 = CARTESIAN_POINT('',(30.2,42.7901059033638,38.49636814359)) ;
#16578 = CARTESIAN_POINT('',(33.6,42.7901059033638,38.49636814359)) ;
#16579 = CARTESIAN_POINT('',(30.2,43.288212014249,38.5491914556663)) ;
#16580 = CARTESIAN_POINT('Origin',(30.2,43.0015367430406,38.4194136113417)) ;
#16581 = CARTESIAN_POINT('',(30.2,42.7901059033638,38.49636814359)) ;
#16582 = CARTESIAN_POINT('Origin',(33.6,43.1377231511858,38.1357267025205)) ;
#16583 = CARTESIAN_POINT('Ctrl Pts',(33.2,42.9053907954888,38.3767638665007)) ;
#16584 = CARTESIAN_POINT('Ctrl Pts',(33.2770142912009,42.8464861060817,38.437875540926)) ;
#16585 = CARTESIAN_POINT('Ctrl Pts',(33.35,42.7901059033638,38.49636814359)) ;
#16586 = CARTESIAN_POINT('Origin',(33.6,42.9412415963219,39.0604142285467)) ;
#16587 = CARTESIAN_POINT('',(33.35,42.9412415963219,39.0604142285467)) ;
#16588 = CARTESIAN_POINT('Ctrl Pts',(33.35,42.9412415963219,39.0604142285467)) ;
#16589 = CARTESIAN_POINT('Ctrl Pts',(33.2770142912008,43.0193145854782,39.0828802070282)) ;
#16590 = CARTESIAN_POINT('Ctrl Pts',(33.2,43.1008833801193,39.1063521248448)) ;
#16591 = CARTESIAN_POINT('',(30.2,42.9412415963219,39.0604142285467)) ;
#16592 = CARTESIAN_POINT('',(33.6,42.9412415963219,39.0604142285467)) ;
#16593 = CARTESIAN_POINT('',(30.2,43.4226076842641,39.1989302542593)) ;
#16594 = CARTESIAN_POINT('Origin',(30.2,43.1628233407496,39.0213433885717)) ;
#16595 = CARTESIAN_POINT('',(30.2,42.9412415963219,39.0604142285467)) ;
#16596 = CARTESIAN_POINT('Origin',(33.6,43.3462024860906,38.7656148429339)) ;
#16597 = CARTESIAN_POINT('Ctrl Pts',(33.2,43.0755441166495,38.9626460206059)) ;
#16598 = CARTESIAN_POINT('Ctrl Pts',(33.2770142912008,43.0069223909346,39.0126005794078)) ;
#16599 = CARTESIAN_POINT('Ctrl Pts',(33.35,42.9412415963219,39.0604142285467)) ;
#16600 = CARTESIAN_POINT('Origin',(33.6,42.992135623731,39.642135623731)) ;
#16601 = CARTESIAN_POINT('',(33.35,42.992135623731,39.642135623731)) ;
#16602 = CARTESIAN_POINT('Ctrl Pts',(33.35,42.992135623731,39.642135623731)) ;
#16603 = CARTESIAN_POINT('Ctrl Pts',(33.2770142912007,43.0651213325302,39.6778175258106)) ;
#16604 = CARTESIAN_POINT('Ctrl Pts',(33.2,43.1413750581413,39.7150971249983)) ;
#16605 = CARTESIAN_POINT('',(30.2,42.992135623731,39.642135623731)) ;
#16606 = CARTESIAN_POINT('',(33.6,42.992135623731,39.642135623731)) ;
#16607 = CARTESIAN_POINT('',(30.2,43.4421356237309,39.8621356237309)) ;
#16608 = CARTESIAN_POINT('Origin',(30.2,43.2171356237309,39.642135623731)) ;
#16609 = CARTESIAN_POINT('',(30.2,42.992135623731,39.642135623731)) ;
#16610 = CARTESIAN_POINT('Origin',(33.6,43.4421356237309,39.422135623731)) ;
#16611 = CARTESIAN_POINT('Ctrl Pts',(33.2,43.1413750581413,39.5691741224637)) ;
#16612 = CARTESIAN_POINT('Ctrl Pts',(33.2770142912006,43.0651213325304,39.6064537216512)) ;
#16613 = CARTESIAN_POINT('Ctrl Pts',(33.35,42.992135623731,39.642135623731)) ;
#16614 = CARTESIAN_POINT('Origin',(29.8,39.642135623731,39.642135623731)) ;
#16615 = CARTESIAN_POINT('Origin',(29.8,39.642135623731,42.9421356237309)) ;
#16616 = CARTESIAN_POINT('Origin',(33.4,39.642135623731,39.642135623731)) ;
#16617 = CARTESIAN_POINT('',(33.6,39.642135623731,42.742135623731)) ;
#16618 = CARTESIAN_POINT('Origin',(33.6,39.642135623731,39.642135623731)) ;
#16619 = CARTESIAN_POINT('',(33.4,39.642135623731,42.9421356237309)) ;
#16620 = CARTESIAN_POINT('Origin',(33.6,39.642135623731,39.642135623731)) ;
#16621 = CARTESIAN_POINT('',(33.6,37.6600848161621,39.6421356)) ;
#16622 = CARTESIAN_POINT('Origin',(33.6,39.642135623731,39.6421356)) ;
#16623 = CARTESIAN_POINT('Origin',(33.45,39.642135623731,39.6421356)) ;
#16624 = CARTESIAN_POINT('',(33.3,38.8810214088786,41.142135623731)) ;
#16625 = CARTESIAN_POINT('',(33.3500000205516,38.7761102199465,41.142135623731)) ;
#16626 = CARTESIAN_POINT('Ctrl Pts',(33.3,38.8810214088786,41.142135623731)) ;
#16627 = CARTESIAN_POINT('Ctrl Pts',(33.3233881136867,38.8293340343079,41.142135623731)) ;
#16628 = CARTESIAN_POINT('Ctrl Pts',(33.3500000205516,38.7761102199465,41.142135623731)) ;
#16629 = CARTESIAN_POINT('',(33.3,40.4032498385833,41.142135623731)) ;
#16630 = CARTESIAN_POINT('Origin',(33.3,39.642135623731,39.6421356)) ;
#16631 = CARTESIAN_POINT('',(33.3500000205516,40.5081610275154,41.142135623731)) ;
#16632 = CARTESIAN_POINT('Ctrl Pts',(33.3500000205516,40.5081610275154,41.142135623731)) ;
#16633 = CARTESIAN_POINT('Ctrl Pts',(33.3233881136867,40.454937213154,41.142135623731)) ;
#16634 = CARTESIAN_POINT('Ctrl Pts',(33.3,40.4032498385833,41.142135623731)) ;
#16635 = CARTESIAN_POINT('',(33.3,40.560616620565,41.0512798714278)) ;
#16636 = CARTESIAN_POINT('Ctrl Pts',(33.3,40.5606166205651,41.0512798714278)) ;
#16637 = CARTESIAN_POINT('Ctrl Pts',(33.3233881137737,40.5347729339775,41.0960424496522)) ;
#16638 = CARTESIAN_POINT('Ctrl Pts',(33.3500000205516,40.5081610275154,41.142135623731)) ;
#16639 = CARTESIAN_POINT('',(33.3,41.3217308588018,39.7329913404377)) ;
#16640 = CARTESIAN_POINT('Origin',(33.3,39.642135623731,39.6421356)) ;
#16641 = CARTESIAN_POINT('',(33.35,41.3741864312998,39.642135623731)) ;
#16642 = CARTESIAN_POINT('Ctrl Pts',(33.35,41.3741864312998,39.642135623731)) ;
#16643 = CARTESIAN_POINT('Ctrl Pts',(33.3233881047513,41.3475745354196,39.6882287794813)) ;
#16644 = CARTESIAN_POINT('Ctrl Pts',(33.3,41.3217308588018,39.7329913404377)) ;
#16645 = CARTESIAN_POINT('',(33.3,41.3217308616346,39.5512799119308)) ;
#16646 = CARTESIAN_POINT('Ctrl Pts',(33.3,41.3217308616346,39.5512799119308)) ;
#16647 = CARTESIAN_POINT('Ctrl Pts',(33.3233881049254,41.3475745368567,39.5960424704698)) ;
#16648 = CARTESIAN_POINT('Ctrl Pts',(33.35,41.3741864312998,39.642135623731)) ;
#16649 = CARTESIAN_POINT('',(33.3,40.560616576629,38.2329912999347)) ;
#16650 = CARTESIAN_POINT('Origin',(33.3,39.642135623731,39.6421356)) ;
#16651 = CARTESIAN_POINT('',(33.3499999794484,40.5081610275154,38.142135623731)) ;
#16652 = CARTESIAN_POINT('Ctrl Pts',(33.3499999794484,40.5081610275154,38.142135623731)) ;
#16653 = CARTESIAN_POINT('Ctrl Pts',(33.3233880959029,40.5347729113766,38.1882287586638)) ;
#16654 = CARTESIAN_POINT('Ctrl Pts',(33.3,40.560616576629,38.2329912999347)) ;
#16655 = CARTESIAN_POINT('',(33.3,40.4032499321209,38.142135623731)) ;
#16656 = CARTESIAN_POINT('Ctrl Pts',(33.3,40.4032499321209,38.142135623731)) ;
#16657 = CARTESIAN_POINT('Ctrl Pts',(33.3233880959899,40.45493726123,38.142135623731)) ;
#16658 = CARTESIAN_POINT('Ctrl Pts',(33.3499999794484,40.5081610275154,38.142135623731)) ;
#16659 = CARTESIAN_POINT('',(33.3,38.881021315341,38.142135623731)) ;
#16660 = CARTESIAN_POINT('Origin',(33.3,39.642135623731,39.6421356)) ;
#16661 = CARTESIAN_POINT('',(33.3499999794484,38.7761102199465,38.142135623731)) ;
#16662 = CARTESIAN_POINT('Ctrl Pts',(33.3499999794484,38.7761102199465,38.142135623731)) ;
#16663 = CARTESIAN_POINT('Ctrl Pts',(33.32338809599,38.8293339862319,38.142135623731)) ;
#16664 = CARTESIAN_POINT('Ctrl Pts',(33.3,38.881021315341,38.142135623731)) ;
#16665 = CARTESIAN_POINT('',(33.3,38.7236546708329,38.2329912999347)) ;
#16666 = CARTESIAN_POINT('Ctrl Pts',(33.3,38.7236546708329,38.2329912999347)) ;
#16667 = CARTESIAN_POINT('Ctrl Pts',(33.3233880959029,38.7494983360852,38.1882287586638)) ;
#16668 = CARTESIAN_POINT('Ctrl Pts',(33.3499999794484,38.7761102199465,38.1421356237309)) ;
#16669 = CARTESIAN_POINT('',(33.3,37.9625403858273,39.5512799119308)) ;
#16670 = CARTESIAN_POINT('Origin',(33.3,39.642135623731,39.6421356)) ;
#16671 = CARTESIAN_POINT('',(33.35,37.9100848161621,39.642135623731)) ;
#16672 = CARTESIAN_POINT('Ctrl Pts',(33.35,37.9100848161621,39.642135623731)) ;
#16673 = CARTESIAN_POINT('Ctrl Pts',(33.3233881049254,37.9366967106052,39.5960424704698)) ;
#16674 = CARTESIAN_POINT('Ctrl Pts',(33.3,37.9625403858273,39.5512799119308)) ;
#16675 = CARTESIAN_POINT('',(33.45,37.8100848161621,39.6421356)) ;
#16676 = CARTESIAN_POINT('',(33.3,37.9625403886601,39.7329913404377)) ;
#16677 = CARTESIAN_POINT('Ctrl Pts',(33.3,37.9625403886601,39.7329913404377)) ;
#16678 = CARTESIAN_POINT('Ctrl Pts',(33.3233881047512,37.9366967120424,39.6882287794813)) ;
#16679 = CARTESIAN_POINT('Ctrl Pts',(33.35,37.9100848161621,39.6421356237309)) ;
#16680 = CARTESIAN_POINT('',(33.3,38.7236546268969,41.0512798714278)) ;
#16681 = CARTESIAN_POINT('Origin',(33.3,39.642135623731,39.6421356)) ;
#16682 = CARTESIAN_POINT('Ctrl Pts',(33.3500000205516,38.7761102199465,41.142135623731)) ;
#16683 = CARTESIAN_POINT('Ctrl Pts',(33.3233881137737,38.7494983134844,41.0960424496523)) ;
#16684 = CARTESIAN_POINT('Ctrl Pts',(33.3,38.7236546268969,41.0512798714278)) ;
#16685 = CARTESIAN_POINT('Origin',(33.45,39.642135623731,39.6421356)) ;
#16686 = CARTESIAN_POINT('',(33.6,38.881021315341,38.142135623731)) ;
#16687 = CARTESIAN_POINT('',(33.45,38.881021315341,38.142135623731)) ;
#16688 = CARTESIAN_POINT('',(33.6,40.4032499321209,38.142135623731)) ;
#16689 = CARTESIAN_POINT('',(33.45,40.4032499321209,38.142135623731)) ;
#16690 = CARTESIAN_POINT('Origin',(33.6,39.642135623731,39.6421356)) ;
#16691 = CARTESIAN_POINT('Origin',(33.45,39.642135623731,39.6421356)) ;
#16692 = CARTESIAN_POINT('',(33.6,41.3217308616346,39.5512799119308)) ;
#16693 = CARTESIAN_POINT('',(33.45,41.3217308616346,39.5512799119308)) ;
#16694 = CARTESIAN_POINT('',(33.6,40.560616576629,38.2329912999347)) ;
#16695 = CARTESIAN_POINT('Origin',(33.6,39.642135623731,39.6421356)) ;
#16696 = CARTESIAN_POINT('',(33.45,40.560616576629,38.2329912999347)) ;
#16697 = CARTESIAN_POINT('Origin',(33.45,39.642135623731,39.6421356)) ;
#16698 = CARTESIAN_POINT('',(33.6,37.9625403858273,39.5512799119308)) ;
#16699 = CARTESIAN_POINT('',(33.45,37.9625403858273,39.5512799119308)) ;
#16700 = CARTESIAN_POINT('',(33.6,38.7236546708329,38.2329912999347)) ;
#16701 = CARTESIAN_POINT('',(33.45,38.7236546708329,38.2329912999347)) ;
#16702 = CARTESIAN_POINT('Origin',(33.6,39.642135623731,39.6421356)) ;
#16703 = CARTESIAN_POINT('Origin',(33.45,39.642135623731,39.6421356)) ;
#16704 = CARTESIAN_POINT('',(33.6,40.560616620565,41.0512798714278)) ;
#16705 = CARTESIAN_POINT('',(33.45,40.560616620565,41.0512798714278)) ;
#16706 = CARTESIAN_POINT('',(33.6,41.3217308588018,39.7329913404377)) ;
#16707 = CARTESIAN_POINT('Origin',(33.6,39.642135623731,39.6421356)) ;
#16708 = CARTESIAN_POINT('',(33.45,41.3217308588018,39.7329913404377)) ;
#16709 = CARTESIAN_POINT('Origin',(33.45,39.642135623731,39.6421356)) ;
#16710 = CARTESIAN_POINT('',(33.6,38.7236546268969,41.0512798714278)) ;
#16711 = CARTESIAN_POINT('',(33.45,38.7236546268969,41.0512798714278)) ;
#16712 = CARTESIAN_POINT('',(33.6,37.9625403886601,39.7329913404377)) ;
#16713 = CARTESIAN_POINT('',(33.45,37.9625403886601,39.7329913404377)) ;
#16714 = CARTESIAN_POINT('Origin',(33.6,39.642135623731,39.6421356)) ;
#16715 = CARTESIAN_POINT('Origin',(33.45,39.642135623731,39.6421356)) ;
#16716 = CARTESIAN_POINT('',(33.6,38.8810214088786,41.142135623731)) ;
#16717 = CARTESIAN_POINT('',(33.45,38.8810214088786,41.142135623731)) ;
#16718 = CARTESIAN_POINT('',(33.6,40.4032498385833,41.142135623731)) ;
#16719 = CARTESIAN_POINT('Origin',(33.6,39.642135623731,39.6421356)) ;
#16720 = CARTESIAN_POINT('',(33.45,40.4032498385833,41.142135623731)) ;
#16721 = CARTESIAN_POINT('Origin',(33.6,37.9100848161621,39.642135623731)) ;
#16722 = CARTESIAN_POINT('',(33.6,38.1265911671082,40.017135623731)) ;
#16723 = CARTESIAN_POINT('',(31.6,37.9100848161621,39.642135623731)) ;
#16724 = CARTESIAN_POINT('',(33.6,37.9100848161621,39.642135623731)) ;
#16725 = CARTESIAN_POINT('',(31.6,38.7761102199465,41.142135623731)) ;
#16726 = CARTESIAN_POINT('',(31.6,38.7761102199465,41.142135623731)) ;
#16727 = CARTESIAN_POINT('',(33.6,38.7761102199465,41.142135623731)) ;
#16728 = CARTESIAN_POINT('Origin',(33.6,38.7761102199465,38.142135623731)) ;
#16729 = CARTESIAN_POINT('',(33.6,38.5596038690004,38.517135623731)) ;
#16730 = CARTESIAN_POINT('',(31.6,38.7761102199465,38.142135623731)) ;
#16731 = CARTESIAN_POINT('',(33.6,38.7761102199465,38.142135623731)) ;
#16732 = CARTESIAN_POINT('',(31.6,37.9100848161621,39.642135623731)) ;
#16733 = CARTESIAN_POINT('Origin',(33.6,40.5081610275154,38.142135623731)) ;
#16734 = CARTESIAN_POINT('',(33.6,40.0751483256232,38.142135623731)) ;
#16735 = CARTESIAN_POINT('',(31.6,40.5081610275154,38.142135623731)) ;
#16736 = CARTESIAN_POINT('',(33.6,40.5081610275154,38.142135623731)) ;
#16737 = CARTESIAN_POINT('',(31.6,38.7761102199465,38.142135623731)) ;
#16738 = CARTESIAN_POINT('Origin',(33.6,39.642135623731,39.642135623731)) ;
#16739 = CARTESIAN_POINT('Origin',(33.6,39.642135623731,39.642135623731)) ;
#16740 = CARTESIAN_POINT('Origin',(33.6,39.642135623731,39.642135623731)) ;
#16741 = CARTESIAN_POINT('',(33.6,41.1576800803537,39.267135623731)) ;
#16742 = CARTESIAN_POINT('Origin',(33.6,39.642135623731,39.642135623731)) ;
#16743 = CARTESIAN_POINT('Origin',(33.6,39.642135623731,39.642135623731)) ;
#16744 = CARTESIAN_POINT('',(33.6,40.7246673784615,40.7671356237309)) ;
#16745 = CARTESIAN_POINT('Origin',(33.6,39.642135623731,39.642135623731)) ;
#16746 = CARTESIAN_POINT('',(33.6,39.2091229218387,41.142135623731)) ;
#16747 = CARTESIAN_POINT('Origin',(31.6,39.642135623731,39.6421356)) ;
#16748 = CARTESIAN_POINT('',(31.6,40.5081610275154,41.142135623731)) ;
#16749 = CARTESIAN_POINT('',(31.6,41.3741864312998,39.642135623731)) ;
#16750 = CARTESIAN_POINT('',(31.6,41.3741864312998,39.642135623731)) ;
#16751 = CARTESIAN_POINT('Origin',(31.6,39.642135623731,39.6421356)) ;
#16752 = CARTESIAN_POINT('Origin',(31.6,39.642135623731,39.6421356)) ;
#16753 = CARTESIAN_POINT('',(31.6,40.5081610275154,38.142135623731)) ;
#16754 = CARTESIAN_POINT('Origin',(31.6,39.642135623731,39.6421356)) ;
#16755 = CARTESIAN_POINT('Origin',(31.6,39.642135623731,39.6421356)) ;
#16756 = CARTESIAN_POINT('Origin',(31.6,39.642135623731,39.6421356)) ;
#16757 = CARTESIAN_POINT('Origin',(31.6,39.642135623731,39.6421356)) ;
#16758 = CARTESIAN_POINT('Origin',(31.6,39.642135623731,39.6421356)) ;
#16759 = CARTESIAN_POINT('Origin',(31.6,39.642135623731,39.6421356)) ;
#16760 = CARTESIAN_POINT('Origin',(31.6,39.642135623731,39.6421356)) ;
#16761 = CARTESIAN_POINT('Origin',(31.6,39.642135623731,39.6421356)) ;
#16762 = CARTESIAN_POINT('',(31.6,40.5081610275154,41.142135623731)) ;
#16763 = CARTESIAN_POINT('Origin',(31.6,39.642135623731,39.6421356)) ;
#16764 = CARTESIAN_POINT('Origin',(31.0796394397885,39.642135623731,39.6421356)) ;
#16765 = CARTESIAN_POINT('',(30.559278879577,39.642135623731,39.6421356)) ;
#16766 = CARTESIAN_POINT('',(31.0796394397885,38.7761102199465,39.6421356)) ;
#16767 = CARTESIAN_POINT('Origin',(33.6,40.5081610275154,41.142135623731)) ;
#16768 = CARTESIAN_POINT('',(33.6,40.5081610275154,41.142135623731)) ;
#16769 = CARTESIAN_POINT('',(33.6,41.3741864312998,39.642135623731)) ;
#16770 = CARTESIAN_POINT('Origin',(33.6,38.7761102199465,41.142135623731)) ;
#16771 = CARTESIAN_POINT('Origin',(33.6,41.3741864312998,39.642135623731)) ;
#16772 = CARTESIAN_POINT('',(0.,0.,0.)) ;
#16773 = CARTESIAN_POINT('Origin',(29.1,37.5,25.5)) ;
#16774 = CARTESIAN_POINT('',(29.1,13.5,25.5)) ;
#16775 = CARTESIAN_POINT('Origin',(29.1,25.5,25.5)) ;
#16776 = CARTESIAN_POINT('',(29.1,16.5,25.5)) ;
#16777 = CARTESIAN_POINT('Origin',(29.1,25.5,25.5)) ;
#16778 = CARTESIAN_POINT('Origin',(30.6,25.5,25.5)) ;
#16779 = CARTESIAN_POINT('',(32.1,13.5,25.5)) ;
#16780 = CARTESIAN_POINT('Origin',(32.1,25.5,25.5)) ;
#16781 = CARTESIAN_POINT('',(30.6,13.5,25.5)) ;
#16782 = CARTESIAN_POINT('Origin',(32.1,34.7,25.5)) ;
#16783 = CARTESIAN_POINT('',(32.1,16.3,25.5)) ;
#16784 = CARTESIAN_POINT('Origin',(32.1,25.5,25.5)) ;
#16785 = CARTESIAN_POINT('Origin',(31.65,25.5,25.5)) ;
#16786 = CARTESIAN_POINT('',(31.2,17.45,25.5)) ;
#16787 = CARTESIAN_POINT('',(31.65,16.875,25.5)) ;
#16788 = CARTESIAN_POINT('Origin',(31.2,25.5,25.5)) ;
#16789 = CARTESIAN_POINT('Origin',(30.95,25.5,25.5)) ;
#16790 = CARTESIAN_POINT('',(30.7,17.45,25.5)) ;
#16791 = CARTESIAN_POINT('',(30.95,17.45,25.5)) ;
#16792 = CARTESIAN_POINT('Origin',(30.7,25.5,25.5)) ;
#16793 = CARTESIAN_POINT('Origin',(30.525,25.5,25.5)) ;
#16794 = CARTESIAN_POINT('',(30.35,16.9,25.5)) ;
#16795 = CARTESIAN_POINT('',(30.525,17.175,25.5)) ;
#16796 = CARTESIAN_POINT('Origin',(30.35,25.5,25.5)) ;
#16797 = CARTESIAN_POINT('Origin',(30.175,25.5,25.5)) ;
#16798 = CARTESIAN_POINT('',(30.,17.45,25.5)) ;
#16799 = CARTESIAN_POINT('',(30.175,17.175,25.5)) ;
#16800 = CARTESIAN_POINT('Origin',(30.,25.5,25.5)) ;
#16801 = CARTESIAN_POINT('Origin',(29.8,25.5,25.5)) ;
#16802 = CARTESIAN_POINT('',(29.6,17.45,25.5)) ;
#16803 = CARTESIAN_POINT('',(29.8,17.45,25.5)) ;
#16804 = CARTESIAN_POINT('Origin',(29.6,25.5,25.5)) ;
#16805 = CARTESIAN_POINT('Origin',(29.35,25.5,25.5)) ;
#16806 = CARTESIAN_POINT('',(29.35,16.975,25.5)) ;
#16807 = CARTESIAN_POINT('',(0.,0.,0.)) ;
#16808 = CARTESIAN_POINT('Origin',(27.85,35.6,22.4)) ;
#16809 = CARTESIAN_POINT('',(27.85,35.6,23.25)) ;
#16810 = CARTESIAN_POINT('Origin',(27.85,35.6,22.4)) ;
#16811 = CARTESIAN_POINT('',(29.05,35.6,23.25)) ;
#16812 = CARTESIAN_POINT('',(27.85,35.6,23.25)) ;
#16813 = CARTESIAN_POINT('Origin',(29.05,35.6,22.4)) ;
#16814 = CARTESIAN_POINT('Origin',(27.85,34.4,20.9)) ;
#16815 = CARTESIAN_POINT('',(29.05,35.0538453413928,20.9)) ;
#16816 = CARTESIAN_POINT('',(27.85,35.0538453413928,20.9)) ;
#16817 = CARTESIAN_POINT('',(27.85,35.0538453413928,20.9)) ;
#16818 = CARTESIAN_POINT('',(29.05,34.4,20.9)) ;
#16819 = CARTESIAN_POINT('',(29.05,36.4,20.9)) ;
#16820 = CARTESIAN_POINT('',(27.85,34.4,20.9)) ;
#16821 = CARTESIAN_POINT('',(27.85,34.4,20.9)) ;
#16822 = CARTESIAN_POINT('',(27.85,36.4,20.9)) ;
#16823 = CARTESIAN_POINT('Origin',(27.85,34.4,24.)) ;
#16824 = CARTESIAN_POINT('',(27.85,34.4,24.)) ;
#16825 = CARTESIAN_POINT('',(27.85,34.4,20.9)) ;
#16826 = CARTESIAN_POINT('',(29.05,34.4,24.)) ;
#16827 = CARTESIAN_POINT('',(29.05,34.4,20.9)) ;
#16828 = CARTESIAN_POINT('',(27.85,34.4,24.)) ;
#16829 = CARTESIAN_POINT('Origin',(27.85,34.5,24.)) ;
#16830 = CARTESIAN_POINT('',(29.05,37.9600361155175,24.)) ;
#16831 = CARTESIAN_POINT('',(29.05,34.4,24.)) ;
#16832 = CARTESIAN_POINT('',(27.85,37.9600361155175,24.)) ;
#16833 = CARTESIAN_POINT('',(27.85,37.9600361155175,24.)) ;
#16834 = CARTESIAN_POINT('',(27.85,30.,24.)) ;
#16835 = CARTESIAN_POINT('Origin',(29.05,25.5,25.5)) ;
#16836 = CARTESIAN_POINT('',(29.05,35.0538453413928,30.1)) ;
#16837 = CARTESIAN_POINT('Origin',(29.05,25.95,25.5)) ;
#16838 = CARTESIAN_POINT('',(29.05,34.4,30.1)) ;
#16839 = CARTESIAN_POINT('',(29.05,36.4,30.1)) ;
#16840 = CARTESIAN_POINT('',(29.05,34.4,27.)) ;
#16841 = CARTESIAN_POINT('',(29.05,34.4,30.1)) ;
#16842 = CARTESIAN_POINT('',(29.05,37.9600361155175,27.)) ;
#16843 = CARTESIAN_POINT('',(29.05,32.,27.)) ;
#16844 = CARTESIAN_POINT('Origin',(29.05,25.5,25.5)) ;
#16845 = CARTESIAN_POINT('',(29.05,35.6,29.45)) ;
#16846 = CARTESIAN_POINT('Origin',(29.05,35.6,28.6)) ;
#16847 = CARTESIAN_POINT('Origin',(27.85,35.6,28.6)) ;
#16848 = CARTESIAN_POINT('',(27.85,35.6,29.45)) ;
#16849 = CARTESIAN_POINT('Origin',(27.85,35.6,28.6)) ;
#16850 = CARTESIAN_POINT('',(27.85,35.6,29.45)) ;
#16851 = CARTESIAN_POINT('Origin',(27.85,36.4,30.1)) ;
#16852 = CARTESIAN_POINT('',(27.85,35.0538453413928,30.1)) ;
#16853 = CARTESIAN_POINT('',(27.85,35.0538453413928,30.1)) ;
#16854 = CARTESIAN_POINT('',(27.85,34.4,30.1)) ;
#16855 = CARTESIAN_POINT('',(27.85,36.4,30.1)) ;
#16856 = CARTESIAN_POINT('',(27.85,34.4,30.1)) ;
#16857 = CARTESIAN_POINT('Origin',(27.85,34.4,30.1)) ;
#16858 = CARTESIAN_POINT('',(27.85,34.4,27.)) ;
#16859 = CARTESIAN_POINT('',(27.85,34.4,30.1)) ;
#16860 = CARTESIAN_POINT('',(27.85,34.4,27.)) ;
#16861 = CARTESIAN_POINT('Origin',(27.85,25.95,25.5)) ;
#16862 = CARTESIAN_POINT('Origin',(27.85,25.95,25.5)) ;
#16863 = CARTESIAN_POINT('Origin',(27.85,38.5,27.)) ;
#16864 = CARTESIAN_POINT('',(27.85,37.9600361155175,27.)) ;
#16865 = CARTESIAN_POINT('',(27.85,32.,27.)) ;
#16866 = CARTESIAN_POINT('',(27.85,37.9600361155175,27.)) ;
#16867 = CARTESIAN_POINT('Origin',(27.85,25.5,25.5)) ;
#16868 = CARTESIAN_POINT('Origin',(27.85,25.5,25.5)) ;
#16869 = CARTESIAN_POINT('Origin',(27.85,25.5,25.5)) ;
#16870 = CARTESIAN_POINT('',(0.,0.,0.)) ;
#16871 = CARTESIAN_POINT('',(0.,0.,0.)) ;
#16872 = CARTESIAN_POINT('',(0.,0.,0.)) ;
#16873 = CARTESIAN_POINT('',(0.,0.,0.)) ;
#16874 = CARTESIAN_POINT('',(0.,0.,0.)) ;
#16875 = CARTESIAN_POINT('',(0.,0.,0.)) ;
#16876 = CARTESIAN_POINT('',(0.,0.,0.)) ;
#16877 = CARTESIAN_POINT('',(3.25,0.,0.)) ;
#16878 = CARTESIAN_POINT('',(6.5,0.,0.)) ;
#16879 = CARTESIAN_POINT('',(9.75,0.,0.)) ;
#16880 = CARTESIAN_POINT('',(13.,0.,0.)) ;
#16881 = CARTESIAN_POINT('',(16.25,0.,0.)) ;
#16882 = CARTESIAN_POINT('',(19.5,0.,0.)) ;
#16883 = CARTESIAN_POINT('',(22.75,0.,0.)) ;
#16884 = CARTESIAN_POINT('',(26.,0.,0.)) ;
#16885 = CARTESIAN_POINT('',(29.25,0.,0.)) ;
#16886 = CARTESIAN_POINT('',(32.5,0.,0.)) ;
#16887 = CARTESIAN_POINT('',(0.,51.,0.)) ;
#16888 = CARTESIAN_POINT('',(3.25,51.,0.)) ;
#16889 = CARTESIAN_POINT('',(6.5,51.,0.)) ;
#16890 = CARTESIAN_POINT('',(9.75,51.,0.)) ;
#16891 = CARTESIAN_POINT('',(13.,51.,0.)) ;
#16892 = CARTESIAN_POINT('',(16.25,51.,0.)) ;
#16893 = CARTESIAN_POINT('',(19.5,51.,0.)) ;
#16894 = CARTESIAN_POINT('',(22.75,51.,0.)) ;
#16895 = CARTESIAN_POINT('',(26.,51.,0.)) ;
#16896 = CARTESIAN_POINT('',(29.25,51.,0.)) ;
#16897 = CARTESIAN_POINT('',(32.5,51.,0.)) ;
#16898 = CARTESIAN_POINT('',(0.,51.,51.)) ;
#16899 = CARTESIAN_POINT('',(3.25,51.,51.)) ;
#16900 = CARTESIAN_POINT('',(6.5,51.,51.)) ;
#16901 = CARTESIAN_POINT('',(9.75,51.,51.)) ;
#16902 = CARTESIAN_POINT('',(13.,51.,51.)) ;
#16903 = CARTESIAN_POINT('',(16.25,51.,51.)) ;
#16904 = CARTESIAN_POINT('',(19.5,51.,51.)) ;
#16905 = CARTESIAN_POINT('',(22.75,51.,51.)) ;
#16906 = CARTESIAN_POINT('',(26.,51.,51.)) ;
#16907 = CARTESIAN_POINT('',(29.25,51.,51.)) ;
#16908 = CARTESIAN_POINT('',(32.5,51.,51.)) ;
#16909 = CARTESIAN_POINT('',(0.,4.44089209850063E-15,51.)) ;
#16910 = CARTESIAN_POINT('',(3.25,4.44089209850063E-15,51.)) ;
#16911 = CARTESIAN_POINT('',(6.5,4.44089209850063E-15,51.)) ;
#16912 = CARTESIAN_POINT('',(9.75,4.44089209850063E-15,51.)) ;
#16913 = CARTESIAN_POINT('',(13.,4.44089209850063E-15,51.)) ;
#16914 = CARTESIAN_POINT('',(16.25,4.44089209850063E-15,51.)) ;
#16915 = CARTESIAN_POINT('',(19.5,4.44089209850063E-15,51.)) ;
#16916 = CARTESIAN_POINT('',(22.75,4.44089209850063E-15,51.)) ;
#16917 = CARTESIAN_POINT('',(26.,4.44089209850063E-15,51.)) ;
#16918 = CARTESIAN_POINT('',(29.25,4.44089209850063E-15,51.)) ;
#16919 = CARTESIAN_POINT('',(32.5,4.44089209850063E-15,51.)) ;
#16920 = CARTESIAN_POINT('',(0.,51.,0.)) ;
#16921 = CARTESIAN_POINT('',(0.,51.,51.)) ;
#16922 = CARTESIAN_POINT('',(0.,4.44089209850063E-15,51.)) ;
#16923 = CARTESIAN_POINT('',(104.,0.,51.)) ;
#16924 = CARTESIAN_POINT('',(104.,0.,51.)) ;
#16925 = UNCERTAINTY_MEASURE_WITH_UNIT(LENGTH_MEASURE(0.01),#16943,
'DISTANCE_ACCURACY_VALUE',
'Maximum model space distance between geometric entities at asserted c
onnectivities') ;
#16926 = UNCERTAINTY_MEASURE_WITH_UNIT(LENGTH_MEASURE(0.01),#16943,
'DISTANCE_ACCURACY_VALUE',
'Maximum model space distance between geometric entities at asserted c
onnectivities') ;
#16927 = UNCERTAINTY_MEASURE_WITH_UNIT(LENGTH_MEASURE(0.01),#16943,
'DISTANCE_ACCURACY_VALUE',
'Maximum model space distance between geometric entities at asserted c
onnectivities') ;
#16928 = UNCERTAINTY_MEASURE_WITH_UNIT(LENGTH_MEASURE(0.01),#16943,
'DISTANCE_ACCURACY_VALUE',
'Maximum model space distance between geometric entities at asserted c
onnectivities') ;
#16929 = UNCERTAINTY_MEASURE_WITH_UNIT(LENGTH_MEASURE(0.01),#16943,
'DISTANCE_ACCURACY_VALUE',
'Maximum model space distance between geometric entities at asserted c
onnectivities') ;
#16930 = UNCERTAINTY_MEASURE_WITH_UNIT(LENGTH_MEASURE(0.01),#16943,
'DISTANCE_ACCURACY_VALUE',
'Maximum model space distance between geometric entities at asserted c
onnectivities') ;
#16931 = UNCERTAINTY_MEASURE_WITH_UNIT(LENGTH_MEASURE(0.01),#16943,
'DISTANCE_ACCURACY_VALUE',
'Maximum model space distance between geometric entities at asserted c
onnectivities') ;
#16932 = UNCERTAINTY_MEASURE_WITH_UNIT(LENGTH_MEASURE(0.01),#16943,
'DISTANCE_ACCURACY_VALUE',
'Maximum model space distance between geometric entities at asserted c
onnectivities') ;
#16933 = UNCERTAINTY_MEASURE_WITH_UNIT(LENGTH_MEASURE(0.01),#16943,
'DISTANCE_ACCURACY_VALUE',
'Maximum model space distance between geometric entities at asserted c
onnectivities') ;
#16934 = (
GEOMETRIC_REPRESENTATION_CONTEXT(3)
GLOBAL_UNCERTAINTY_ASSIGNED_CONTEXT((#16925))
GLOBAL_UNIT_ASSIGNED_CONTEXT((#16943,#16945,#16946))
REPRESENTATION_CONTEXT('','3D')
) ;
#16935 = (
GEOMETRIC_REPRESENTATION_CONTEXT(3)
GLOBAL_UNCERTAINTY_ASSIGNED_CONTEXT((#16926))
GLOBAL_UNIT_ASSIGNED_CONTEXT((#16943,#16945,#16946))
REPRESENTATION_CONTEXT('','3D')
) ;
#16936 = (
GEOMETRIC_REPRESENTATION_CONTEXT(3)
GLOBAL_UNCERTAINTY_ASSIGNED_CONTEXT((#16927))
GLOBAL_UNIT_ASSIGNED_CONTEXT((#16943,#16945,#16946))
REPRESENTATION_CONTEXT('','3D')
) ;
#16937 = (
GEOMETRIC_REPRESENTATION_CONTEXT(3)
GLOBAL_UNCERTAINTY_ASSIGNED_CONTEXT((#16928))
GLOBAL_UNIT_ASSIGNED_CONTEXT((#16943,#16945,#16946))
REPRESENTATION_CONTEXT('','3D')
) ;
#16938 = (
GEOMETRIC_REPRESENTATION_CONTEXT(3)
GLOBAL_UNCERTAINTY_ASSIGNED_CONTEXT((#16929))
GLOBAL_UNIT_ASSIGNED_CONTEXT((#16943,#16945,#16946))
REPRESENTATION_CONTEXT('','3D')
) ;
#16939 = (
GEOMETRIC_REPRESENTATION_CONTEXT(3)
GLOBAL_UNCERTAINTY_ASSIGNED_CONTEXT((#16930))
GLOBAL_UNIT_ASSIGNED_CONTEXT((#16943,#16945,#16946))
REPRESENTATION_CONTEXT('','3D')
) ;
#16940 = (
GEOMETRIC_REPRESENTATION_CONTEXT(3)
GLOBAL_UNCERTAINTY_ASSIGNED_CONTEXT((#16931))
GLOBAL_UNIT_ASSIGNED_CONTEXT((#16943,#16945,#16946))
REPRESENTATION_CONTEXT('','3D')
) ;
#16941 = (
GEOMETRIC_REPRESENTATION_CONTEXT(3)
GLOBAL_UNCERTAINTY_ASSIGNED_CONTEXT((#16932))
GLOBAL_UNIT_ASSIGNED_CONTEXT((#16943,#16945,#16946))
REPRESENTATION_CONTEXT('','3D')
) ;
#16942 = (
GEOMETRIC_REPRESENTATION_CONTEXT(3)
GLOBAL_UNCERTAINTY_ASSIGNED_CONTEXT((#16933))
GLOBAL_UNIT_ASSIGNED_CONTEXT((#16943,#16945,#16946))
REPRESENTATION_CONTEXT('','3D')
) ;
#16943 = (
LENGTH_UNIT()
NAMED_UNIT(*)
SI_UNIT(.MILLI.,.METRE.)
) ;
#16944 = (
LENGTH_UNIT()
NAMED_UNIT(*)
SI_UNIT($,.METRE.)
) ;
#16945 = (
NAMED_UNIT(*)
PLANE_ANGLE_UNIT()
SI_UNIT($,.RADIAN.)
) ;
#16946 = (
NAMED_UNIT(*)
SI_UNIT($,.STERADIAN.)
SOLID_ANGLE_UNIT()
) ;
#16947 = SHAPE_DEFINITION_REPRESENTATION(#16955,#17018) ;
#16948 = SHAPE_DEFINITION_REPRESENTATION(#16956,#17019) ;
#16949 = SHAPE_DEFINITION_REPRESENTATION(#16957,#17020) ;
#16950 = SHAPE_DEFINITION_REPRESENTATION(#16958,#17021) ;
#16951 = SHAPE_DEFINITION_REPRESENTATION(#16959,#17022) ;
#16952 = SHAPE_DEFINITION_REPRESENTATION(#16960,#17023) ;
#16953 = SHAPE_DEFINITION_REPRESENTATION(#16961,#17024) ;
#16954 = SHAPE_DEFINITION_REPRESENTATION(#16962,#17025) ;
#16955 = PRODUCT_DEFINITION_SHAPE('',$,#17027) ;
#16956 = PRODUCT_DEFINITION_SHAPE('',$,#17028) ;
#16957 = PRODUCT_DEFINITION_SHAPE('',$,#17029) ;
#16958 = PRODUCT_DEFINITION_SHAPE('',$,#17030) ;
#16959 = PRODUCT_DEFINITION_SHAPE('',$,#17031) ;
#16960 = PRODUCT_DEFINITION_SHAPE('',$,#17032) ;
#16961 = PRODUCT_DEFINITION_SHAPE('',$,#17033) ;
#16962 = PRODUCT_DEFINITION_SHAPE('',$,#17034) ;
#16963 = PRODUCT_DEFINITION_SHAPE($,$,#176) ;
#16964 = PRODUCT_DEFINITION_SHAPE($,$,#177) ;
#16965 = PRODUCT_DEFINITION_SHAPE($,$,#178) ;
#16966 = PRODUCT_DEFINITION_SHAPE($,$,#179) ;
#16967 = PRODUCT_DEFINITION_SHAPE($,$,#180) ;
#16968 = PRODUCT_DEFINITION_SHAPE($,$,#181) ;
#16969 = PRODUCT_DEFINITION_SHAPE($,$,#182) ;
#16970 = PRODUCT_DEFINITION_SHAPE($,$,#183) ;
#16971 = PRODUCT_DEFINITION_SHAPE($,$,#184) ;
#16972 = PRODUCT_DEFINITION_SHAPE($,$,#185) ;
#16973 = PRODUCT_DEFINITION_SHAPE($,$,#186) ;
#16974 = PRODUCT_DEFINITION_SHAPE($,$,#187) ;
#16975 = PRODUCT_DEFINITION_SHAPE($,$,#188) ;
#16976 = PRODUCT_DEFINITION_SHAPE($,$,#189) ;
#16977 = PRODUCT_DEFINITION_SHAPE($,$,#190) ;
#16978 = PRODUCT_DEFINITION_SHAPE($,$,#191) ;
#16979 = PRODUCT_DEFINITION_SHAPE($,$,#192) ;
#16980 = PRODUCT_DEFINITION_SHAPE($,$,#193) ;
#16981 = PRODUCT_DEFINITION_SHAPE($,$,#194) ;
#16982 = PRODUCT_DEFINITION_SHAPE($,$,#195) ;
#16983 = PRODUCT_DEFINITION_SHAPE($,$,#196) ;
#16984 = PRODUCT_DEFINITION_SHAPE($,$,#197) ;
#16985 = PRODUCT_DEFINITION_SHAPE($,$,#198) ;
#16986 = PRODUCT_DEFINITION_SHAPE($,$,#199) ;
#16987 = PRODUCT_DEFINITION_SHAPE($,$,#200) ;
#16988 = PRODUCT_DEFINITION_SHAPE($,$,#201) ;
#16989 = PRODUCT_DEFINITION_SHAPE($,$,#202) ;
#16990 = PRODUCT_DEFINITION_SHAPE($,$,#203) ;
#16991 = PRODUCT_DEFINITION_SHAPE($,$,#204) ;
#16992 = PRODUCT_DEFINITION_SHAPE($,$,#205) ;
#16993 = PRODUCT_DEFINITION_SHAPE($,$,#206) ;
#16994 = PRODUCT_DEFINITION_SHAPE($,$,#207) ;
#16995 = PRODUCT_DEFINITION_SHAPE($,$,#208) ;
#16996 = PRODUCT_DEFINITION_SHAPE($,$,#209) ;
#16997 = PRODUCT_DEFINITION_SHAPE($,$,#210) ;
#16998 = PRODUCT_DEFINITION_SHAPE($,$,#211) ;
#16999 = PRODUCT_DEFINITION_SHAPE($,$,#212) ;
#17000 = PRODUCT_DEFINITION_SHAPE($,$,#213) ;
#17001 = PRODUCT_DEFINITION_SHAPE($,$,#214) ;
#17002 = PRODUCT_DEFINITION_SHAPE($,$,#215) ;
#17003 = PRODUCT_DEFINITION_SHAPE($,$,#216) ;
#17004 = PRODUCT_DEFINITION_SHAPE($,$,#217) ;
#17005 = PRODUCT_DEFINITION_SHAPE($,$,#218) ;
#17006 = PRODUCT_DEFINITION_SHAPE($,$,#219) ;
#17007 = PRODUCT_DEFINITION_SHAPE($,$,#220) ;
#17008 = PRODUCT_DEFINITION_SHAPE($,$,#221) ;
#17009 = PRODUCT_DEFINITION_SHAPE($,$,#222) ;
#17010 = PRODUCT_DEFINITION_SHAPE($,$,#223) ;
#17011 = PRODUCT_DEFINITION_SHAPE($,$,#224) ;
#17012 = PRODUCT_DEFINITION_SHAPE($,$,#225) ;
#17013 = PRODUCT_DEFINITION_SHAPE($,$,#226) ;
#17014 = PRODUCT_DEFINITION_SHAPE($,$,#227) ;
#17015 = PRODUCT_DEFINITION_SHAPE($,$,#228) ;
#17016 = PRODUCT_DEFINITION_SHAPE($,$,#229) ;
#17017 = PRODUCT_DEFINITION_SHAPE($,$,#230) ;
#17018 = SHAPE_REPRESENTATION('',(#8263,#8917,#8918,#8919,#8920,#8921,#8922,
#8923,#8924,#8925,#8926,#8927,#8928,#8929,#8930,#8931,#8932,#8933,#8934,
#8935,#8936,#8937,#8938,#8939,#8940,#8941,#8942,#8943,#8944,#8945,#8946,
#8947,#8948,#8949,#8950,#8951,#8952,#8953,#8954,#8955,#8956,#8957,#8958,
#8959,#8960,#8961,#8962,#8963,#8964,#8965,#8966,#8967,#8968,#8969,#8970,
#8971),#16934) ;
#17019 = SHAPE_REPRESENTATION('',(#8264),#16935) ;
#17020 = SHAPE_REPRESENTATION('',(#8345),#16936) ;
#17021 = SHAPE_REPRESENTATION('',(#8552),#16937) ;
#17022 = SHAPE_REPRESENTATION('',(#8593),#16938) ;
#17023 = SHAPE_REPRESENTATION('',(#8596),#16939) ;
#17024 = SHAPE_REPRESENTATION('',(#8877),#16940) ;
#17025 = SHAPE_REPRESENTATION('',(#8896),#16941) ;
#17026 = PRODUCT_DEFINITION_CONTEXT('part definition',#17052,'design') ;
#17027 = PRODUCT_DEFINITION('MAS-257','MAS-257',#17035,
#17026) ;
#17028 = PRODUCT_DEFINITION('Ball Spline Shaft No.16 x 120 Stepped D12 Tapped M8',
'Ball Spline Shaft No.16 x 120 Stepped D12 Tapped M8',#17036,#17026) ;
#17029 = PRODUCT_DEFINITION('Ball Spline Nut Outer Sleeve Round Flange BSLM16',
'Ball Spline Nut Outer Sleeve Round Flange BSLM16',#17037,#17026) ;
#17030 = PRODUCT_DEFINITION('Internal Ball Retainer Cage BSLM16',
'Internal Ball Retainer Cage BSLM16',#17038,#17026) ;
#17031 = PRODUCT_DEFINITION('Precision Steel Ball D3.175 G10',
'Precision Steel Ball D3.175 G10',#17039,#17026) ;
#17032 = PRODUCT_DEFINITION('ISO 4762 - M4 x 10 - 12.9',
'ISO 4762 - M4 x 10 - 12.9',#17040,#17026) ;
#17033 = PRODUCT_DEFINITION('Wiper Rubber Seal BSLM16',
'Wiper Rubber Seal BSLM16',#17041,#17026) ;
#17034 = PRODUCT_DEFINITION('DIN 472 - J24 x 1.2 Internal Retaining Ring',
'DIN 472 - J24 x 1.2 Internal Retaining Ring',#17042,#17026) ;
#17035 = PRODUCT_DEFINITION_FORMATION('',$,#17054) ;
#17036 = PRODUCT_DEFINITION_FORMATION('',$,#17055) ;
#17037 = PRODUCT_DEFINITION_FORMATION('',$,#17056) ;
#17038 = PRODUCT_DEFINITION_FORMATION('',$,#17057) ;
#17039 = PRODUCT_DEFINITION_FORMATION('',$,#17058) ;
#17040 = PRODUCT_DEFINITION_FORMATION('',$,#17059) ;
#17041 = PRODUCT_DEFINITION_FORMATION('',$,#17060) ;
#17042 = PRODUCT_DEFINITION_FORMATION('',$,#17061) ;
#17043 = PRODUCT_RELATED_PRODUCT_CATEGORY('MAS-257','MAS-257',(#17054)) ;
#17044 = PRODUCT_RELATED_PRODUCT_CATEGORY(
'Ball Spline Shaft No.16 x 120 Stepped D12 Tapped M8',
'Ball Spline Shaft No.16 x 120 Stepped D12 Tapped M8',(#17055)) ;
#17045 = PRODUCT_RELATED_PRODUCT_CATEGORY(
'Ball Spline Nut Outer Sleeve Round Flange BSLM16',
'Ball Spline Nut Outer Sleeve Round Flange BSLM16',(#17056)) ;
#17046 = PRODUCT_RELATED_PRODUCT_CATEGORY(
'Internal Ball Retainer Cage BSLM16',
'Internal Ball Retainer Cage BSLM16',(#17057)) ;
#17047 = PRODUCT_RELATED_PRODUCT_CATEGORY(
'Precision Steel Ball D3.175 G10','Precision Steel Ball D3.175 G10',(#17058)) ;
#17048 = PRODUCT_RELATED_PRODUCT_CATEGORY('ISO 4762 - M4 x 10 - 12.9',
'ISO 4762 - M4 x 10 - 12.9',(#17059)) ;
#17049 = PRODUCT_RELATED_PRODUCT_CATEGORY('Wiper Rubber Seal BSLM16',
'Wiper Rubber Seal BSLM16',(#17060)) ;
#17050 = PRODUCT_RELATED_PRODUCT_CATEGORY(
'DIN 472 - J24 x 1.2 Internal Retaining Ring',
'DIN 472 - J24 x 1.2 Internal Retaining Ring',(#17061)) ;
#17051 = APPLICATION_PROTOCOL_DEFINITION('international standard',
'automotive_design',2009,#17052) ;
#17052 = APPLICATION_CONTEXT(
'Core Data for Automotive Mechanical Design Process') ;
#17053 = PRODUCT_CONTEXT('part definition',#17052,'mechanical') ;
#17054 = PRODUCT('MAS-257','MAS-257',$,(#17053)) ;
#17055 = PRODUCT('Ball Spline Shaft No.16 x 120 Stepped D12 Tapped M8',
'Ball Spline Shaft No.16 x 120 Stepped D12 Tapped M8',$,(#17053)) ;
#17056 = PRODUCT('Ball Spline Nut Outer Sleeve Round Flange BSLM16',
'Ball Spline Nut Outer Sleeve Round Flange BSLM16',$,(#17053)) ;
#17057 = PRODUCT('Internal Ball Retainer Cage BSLM16',
'Internal Ball Retainer Cage BSLM16',$,(#17053)) ;
#17058 = PRODUCT('Precision Steel Ball D3.175 G10',
'Precision Steel Ball D3.175 G10',$,(#17053)) ;
#17059 = PRODUCT('ISO 4762 - M4 x 10 - 12.9','ISO 4762 - M4 x 10 - 12.9',$,
(#17053)) ;
#17060 = PRODUCT('Wiper Rubber Seal BSLM16','Wiper Rubber Seal BSLM16',$,(#17053)) ;
#17061 = PRODUCT('DIN 472 - J24 x 1.2 Internal Retaining Ring',
'DIN 472 - J24 x 1.2 Internal Retaining Ring',$,(#17053)) ;
#17062 = PRESENTATION_STYLE_ASSIGNMENT((#17070)) ;
#17063 = PRESENTATION_STYLE_ASSIGNMENT((#17071)) ;
#17064 = PRESENTATION_STYLE_ASSIGNMENT((#17072)) ;
#17065 = PRESENTATION_STYLE_ASSIGNMENT((#17073)) ;
#17066 = PRESENTATION_STYLE_ASSIGNMENT((#17074)) ;
#17067 = PRESENTATION_STYLE_ASSIGNMENT((#17075)) ;
#17068 = PRESENTATION_STYLE_ASSIGNMENT((#17076)) ;
#17069 = PRESENTATION_STYLE_ASSIGNMENT((#17077)) ;
#17070 = SURFACE_STYLE_USAGE(.BOTH.,#17078) ;
#17071 = SURFACE_STYLE_USAGE(.BOTH.,#17079) ;
#17072 = SURFACE_STYLE_USAGE(.BOTH.,#17080) ;
#17073 = SURFACE_STYLE_USAGE(.BOTH.,#17081) ;
#17074 = SURFACE_STYLE_USAGE(.BOTH.,#17082) ;
#17075 = SURFACE_STYLE_USAGE(.BOTH.,#17083) ;
#17076 = SURFACE_STYLE_USAGE(.BOTH.,#17084) ;
#17077 = SURFACE_STYLE_USAGE(.BOTH.,#17085) ;
#17078 = SURFACE_SIDE_STYLE('',(#17086)) ;
#17079 = SURFACE_SIDE_STYLE('',(#17087)) ;
#17080 = SURFACE_SIDE_STYLE('',(#17088)) ;
#17081 = SURFACE_SIDE_STYLE('',(#17089)) ;
#17082 = SURFACE_SIDE_STYLE('',(#17090)) ;
#17083 = SURFACE_SIDE_STYLE('',(#17091)) ;
#17084 = SURFACE_SIDE_STYLE('',(#17092)) ;
#17085 = SURFACE_SIDE_STYLE('',(#17093)) ;
#17086 = SURFACE_STYLE_FILL_AREA(#17094) ;
#17087 = SURFACE_STYLE_FILL_AREA(#17095) ;
#17088 = SURFACE_STYLE_FILL_AREA(#17096) ;
#17089 = SURFACE_STYLE_FILL_AREA(#17097) ;
#17090 = SURFACE_STYLE_FILL_AREA(#17098) ;
#17091 = SURFACE_STYLE_FILL_AREA(#17099) ;
#17092 = SURFACE_STYLE_FILL_AREA(#17100) ;
#17093 = SURFACE_STYLE_FILL_AREA(#17101) ;
#17094 = FILL_AREA_STYLE('Steel - Satin',(#17102)) ;
#17095 = FILL_AREA_STYLE(
'MAS-257 Metallic Sheet - Ball Spline Shaft No.16 x 120 Stepped D1',(#17103)) ;
#17096 = FILL_AREA_STYLE(
'MAS-257 Metallic Sheet - Ball Spline Nut Outer Sleeve Round Flang',(#17104)) ;
#17097 = FILL_AREA_STYLE(
'MAS-257 Plastic - Internal Ball Retainer Cage BSLM16',(#17105)) ;
#17098 = FILL_AREA_STYLE(
'MAS-257 Metallic Sheet - Precision Steel Ball D3.175 G10',(#17106)) ;
#17099 = FILL_AREA_STYLE(
'MAS-257 Metallic Sheet - ISO 4762 - M4 x 10 - 12.9',(#17107)) ;
#17100 = FILL_AREA_STYLE('Rubber - Soft',(#17108)) ;
#17101 = FILL_AREA_STYLE(
'MAS-257 Metallic Sheet - DIN 472 - J24 x 1.2 Internal Retaining R',(#17109)) ;
#17102 = FILL_AREA_STYLE_COLOUR('Steel - Satin',#17110) ;
#17103 = FILL_AREA_STYLE_COLOUR(
'MAS-257 Metallic Sheet - Ball Spline Shaft No.16 x 120 Stepped D1',#17111) ;
#17104 = FILL_AREA_STYLE_COLOUR(
'MAS-257 Metallic Sheet - Ball Spline Nut Outer Sleeve Round Flang',#17112) ;
#17105 = FILL_AREA_STYLE_COLOUR(
'MAS-257 Plastic - Internal Ball Retainer Cage BSLM16',#17113) ;
#17106 = FILL_AREA_STYLE_COLOUR(
'MAS-257 Metallic Sheet - Precision Steel Ball D3.175 G10',#17114) ;
#17107 = FILL_AREA_STYLE_COLOUR(
'MAS-257 Metallic Sheet - ISO 4762 - M4 x 10 - 12.9',#17115) ;
#17108 = FILL_AREA_STYLE_COLOUR('Rubber - Soft',#17116) ;
#17109 = FILL_AREA_STYLE_COLOUR(
'MAS-257 Metallic Sheet - DIN 472 - J24 x 1.2 Internal Retaining R',#17117) ;
#17110 = COLOUR_RGB('Steel - Satin', 0.66274510, 0.83137255, 0.94901961) ;
#17111 = COLOUR_RGB(
'MAS-257 Metallic Sheet - Ball Spline Shaft No.16 x 120 Stepped D1', 0.66274510, 0.83137255, 0.94901961) ;
#17112 = COLOUR_RGB(
'MAS-257 Metallic Sheet - Ball Spline Nut Outer Sleeve Round Flang', 0.31764706, 0.68627451, 0.89019608) ;
#17113 = COLOUR_RGB(
'MAS-257 Plastic - Internal Ball Retainer Cage BSLM16', 0.40784314, 0.44705882, 0.49803922) ;
#17114 = COLOUR_RGB(
'MAS-257 Metallic Sheet - Precision Steel Ball D3.175 G10', 0.72549020, 0.75294118, 0.79215686) ;
#17115 = COLOUR_RGB('MAS-257 Metallic Sheet - ISO 4762 - M4 x 10 - 12.9', 0.08235294, 0.09019608, 0.10196078) ;
#17116 = COLOUR_RGB('Rubber - Soft', 0.09019608, 0.27058824, 0.51372549) ;
#17117 = COLOUR_RGB(
'MAS-257 Metallic Sheet - DIN 472 - J24 x 1.2 Internal Retaining R', 0.66274510, 0.83137255, 0.94901961) ;
ENDSEC;
END-ISO-10303-21;
